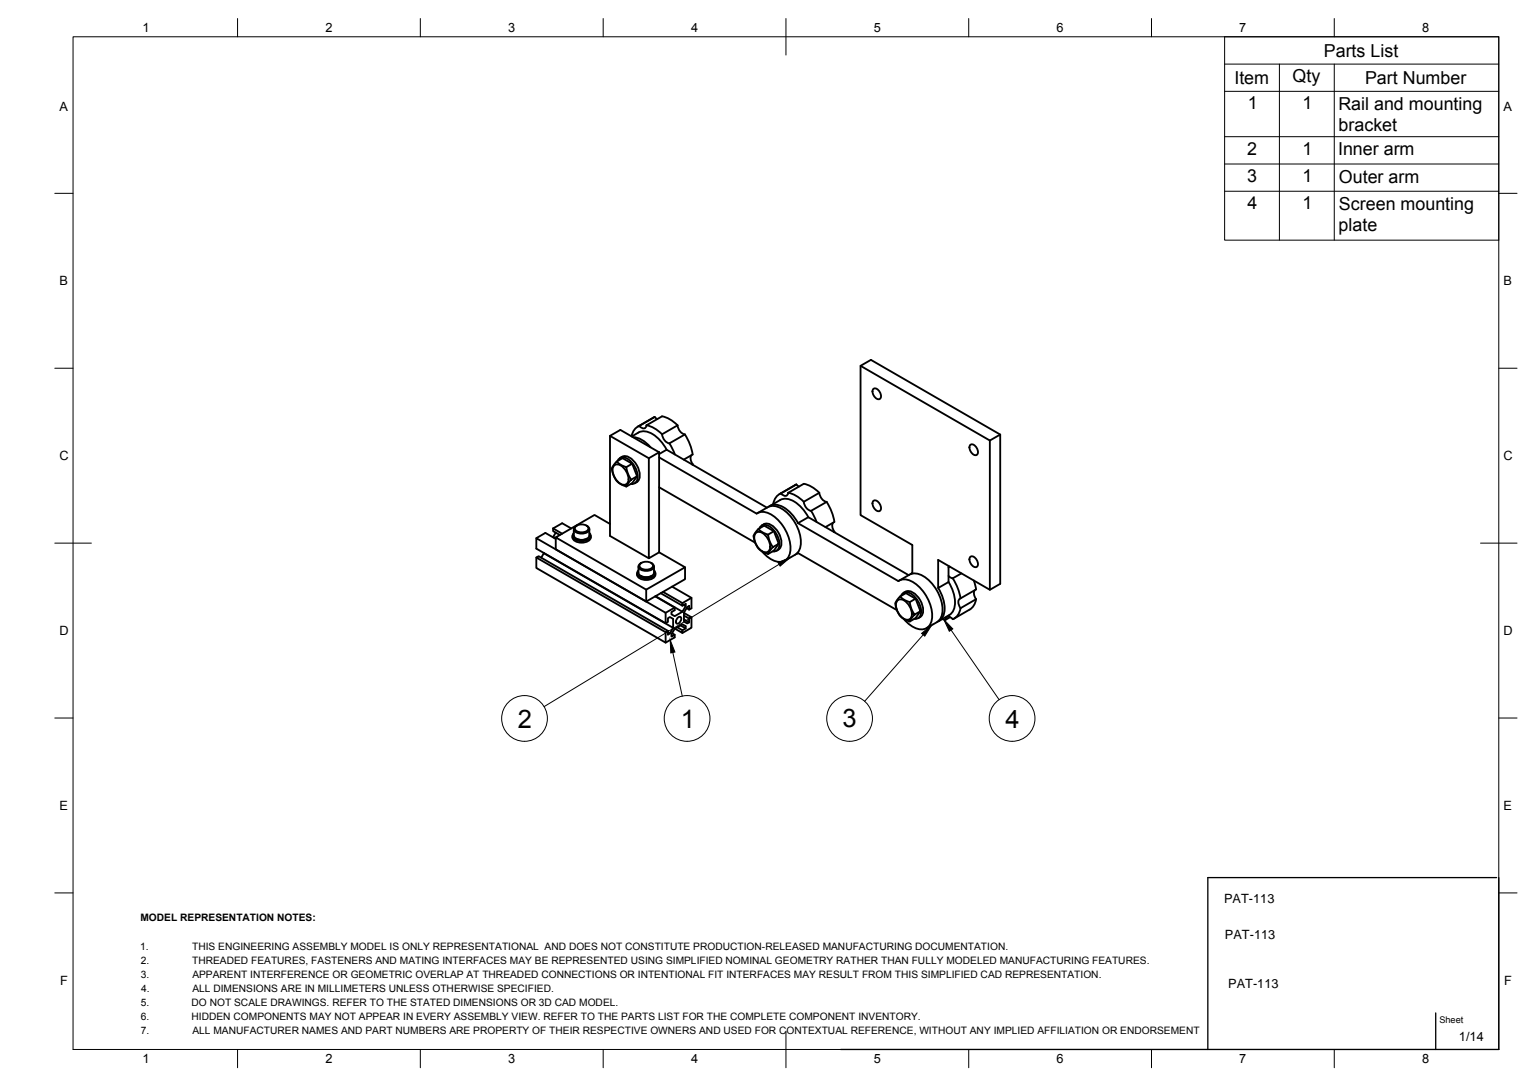
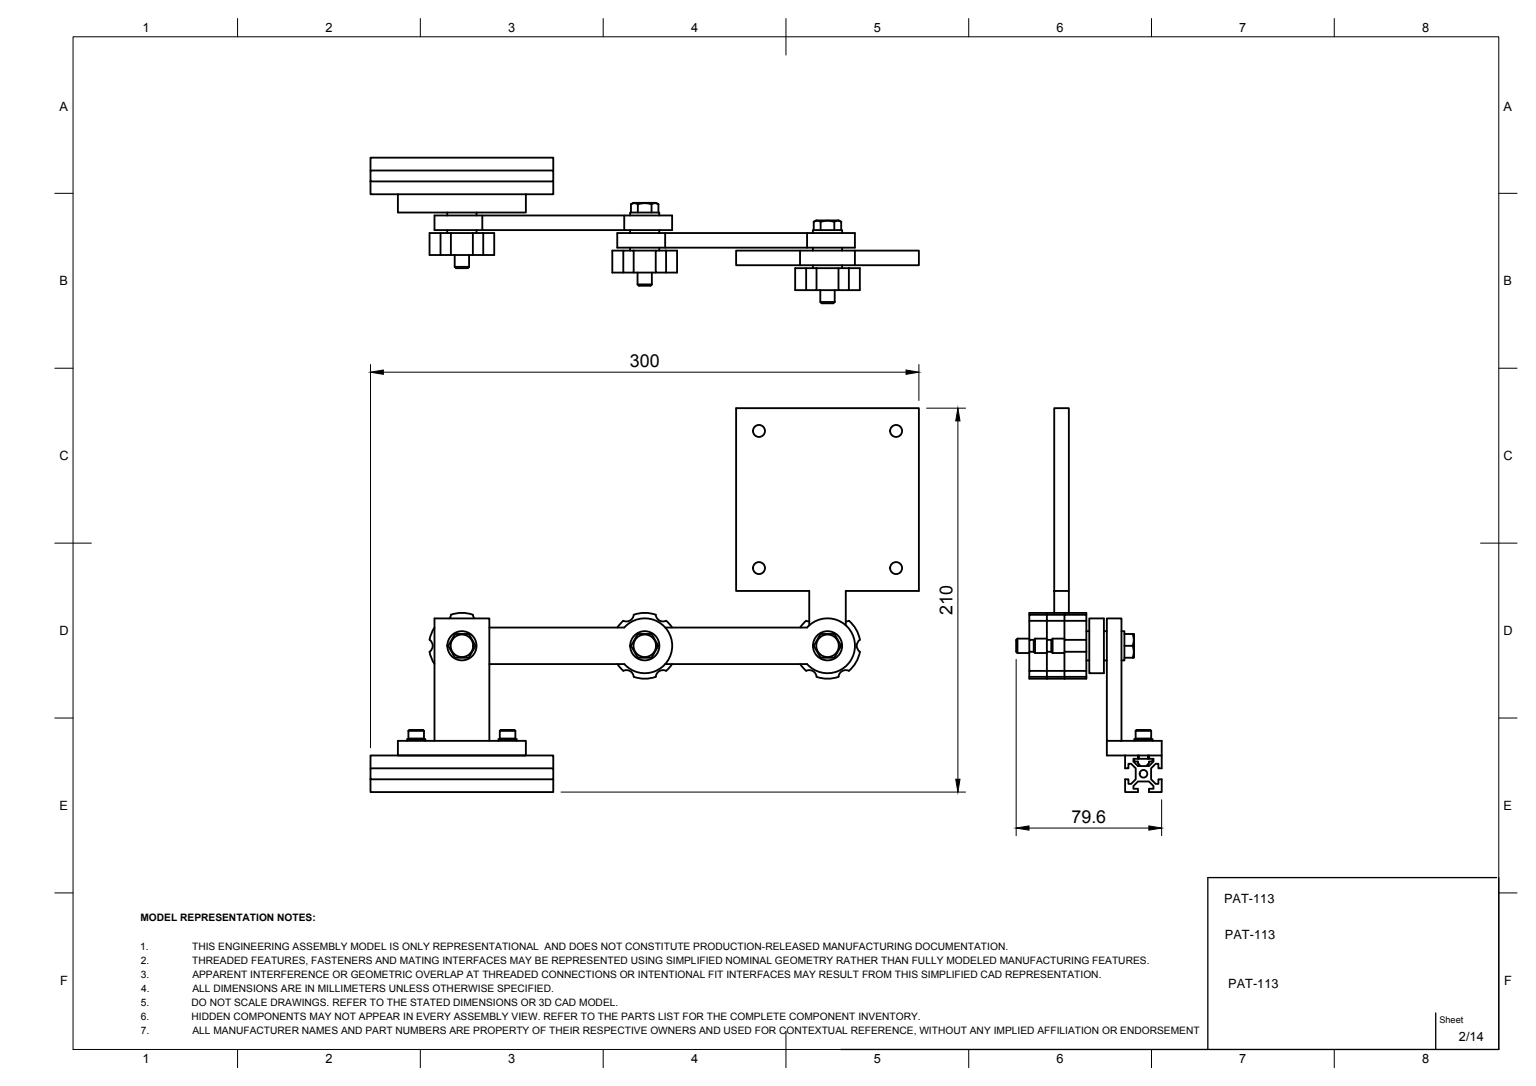
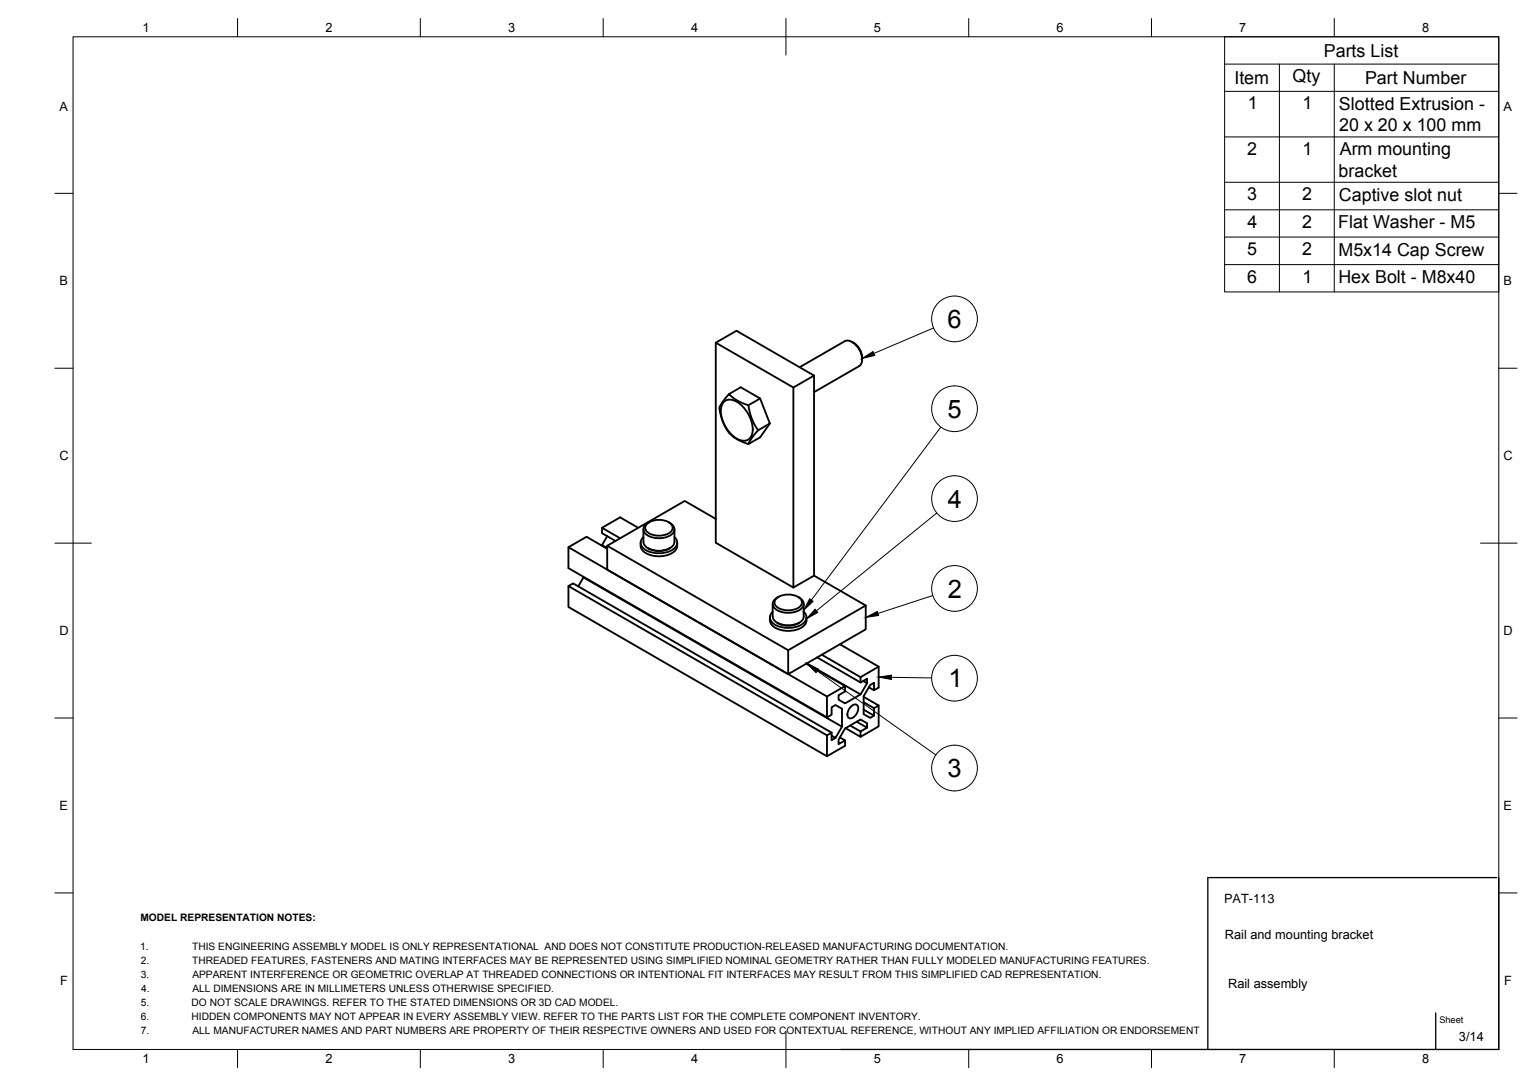
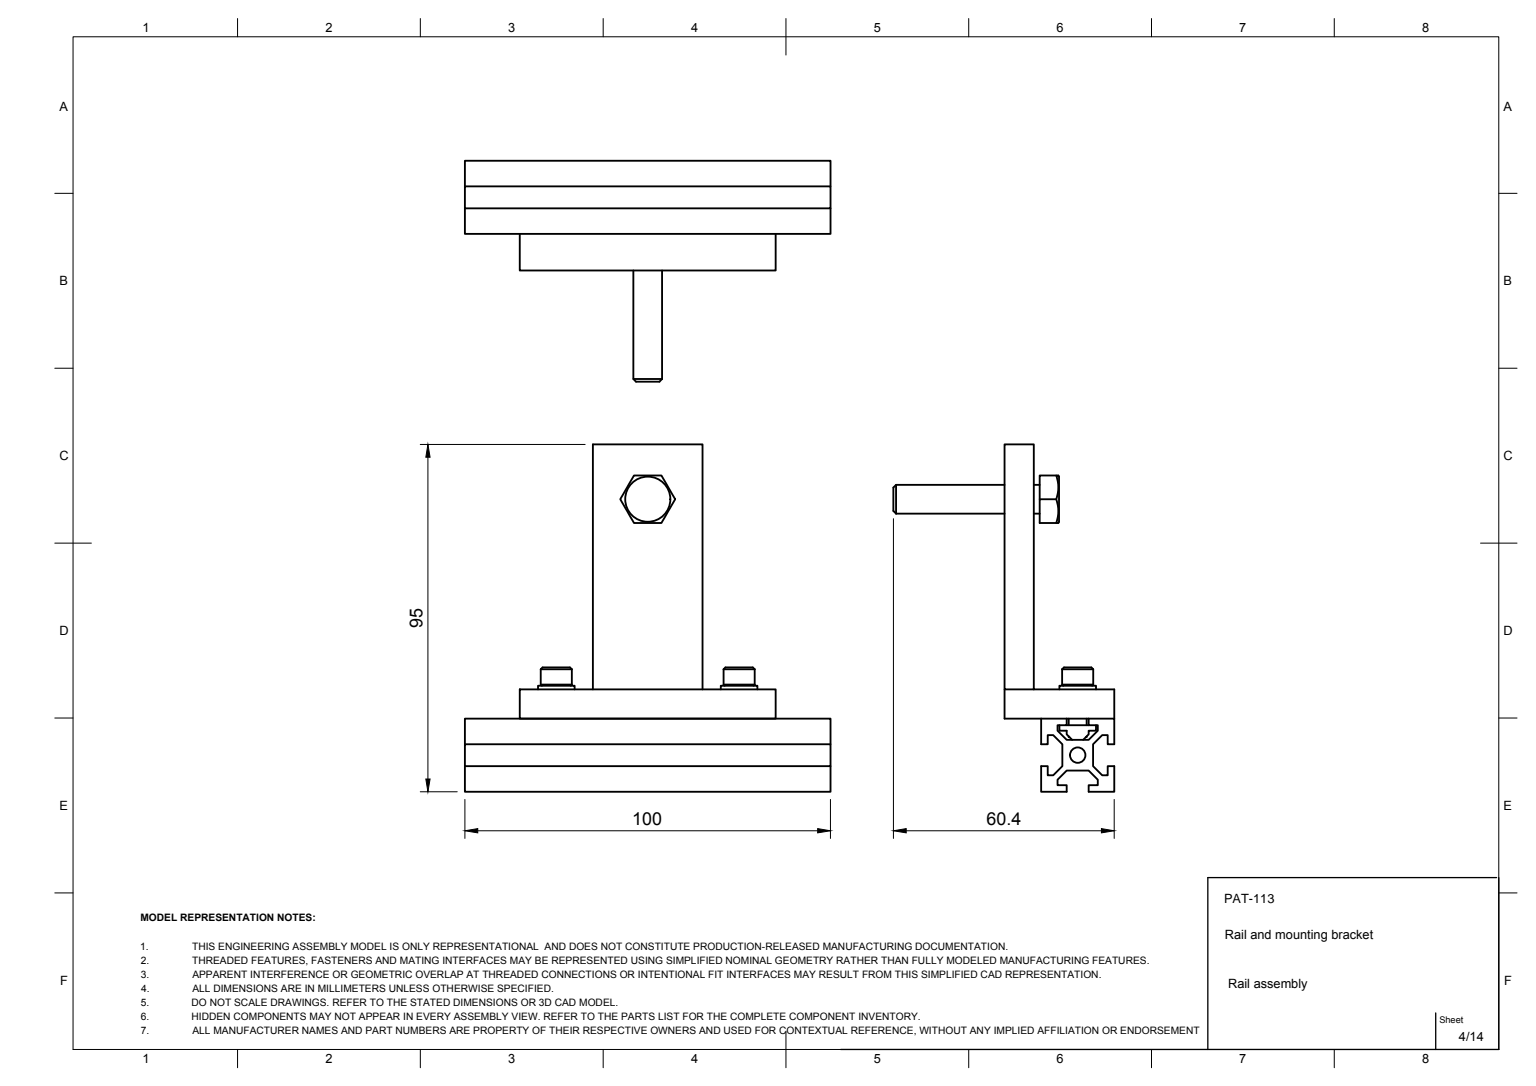
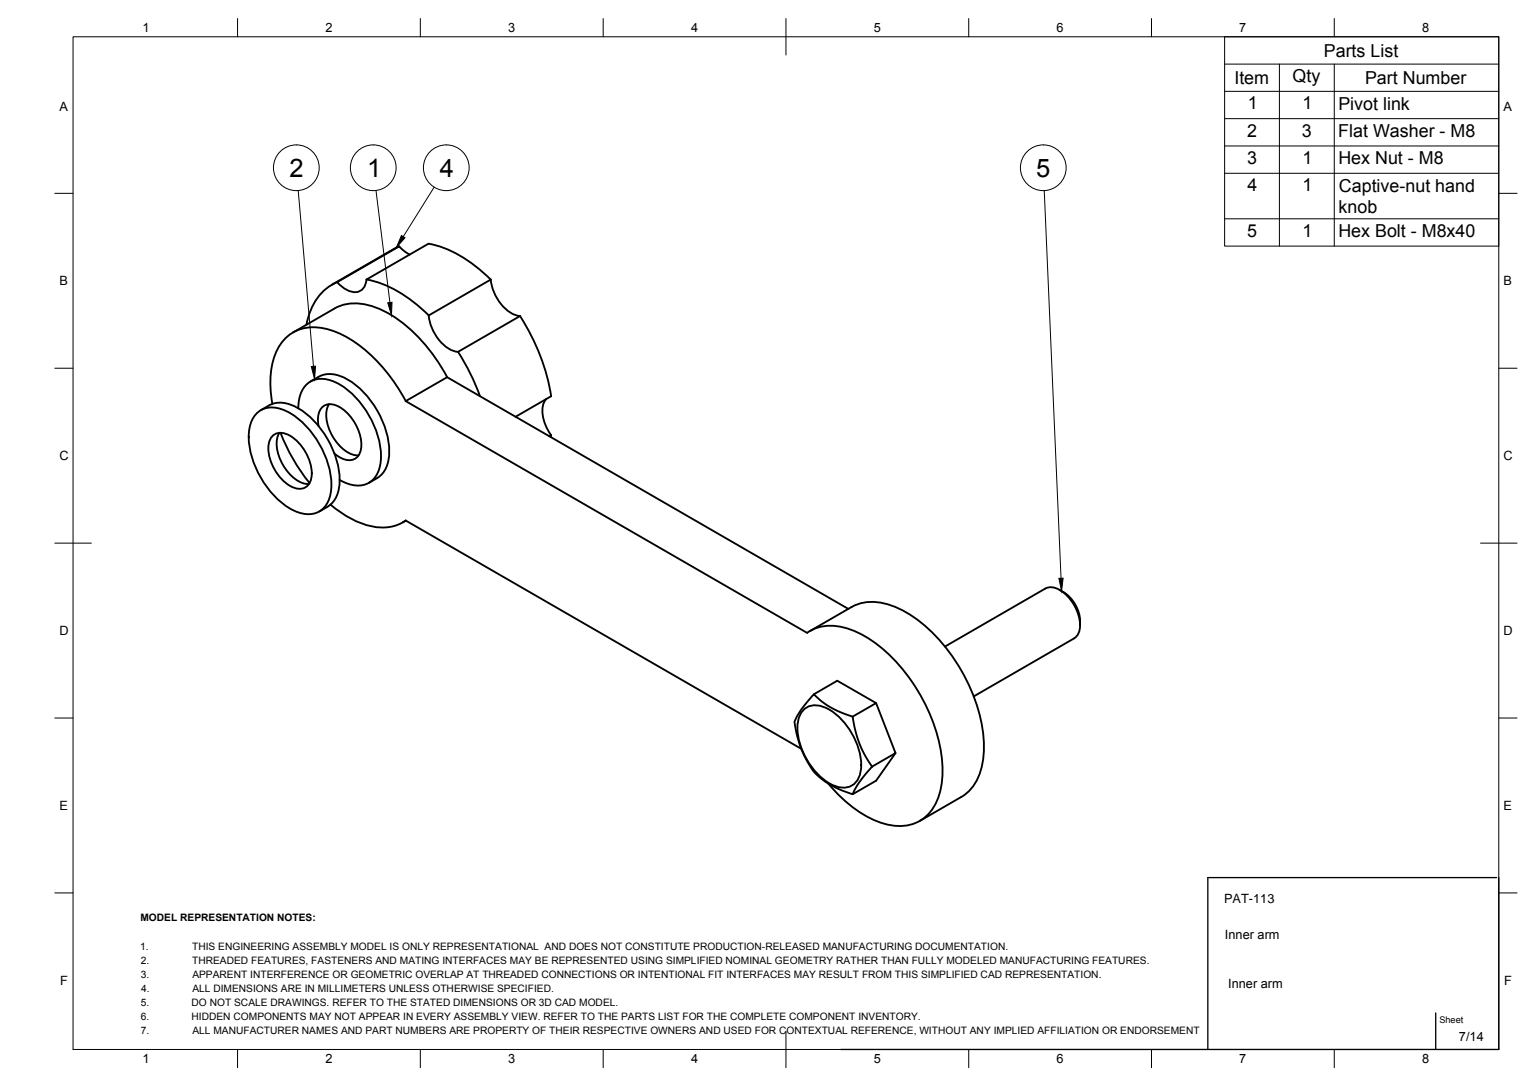
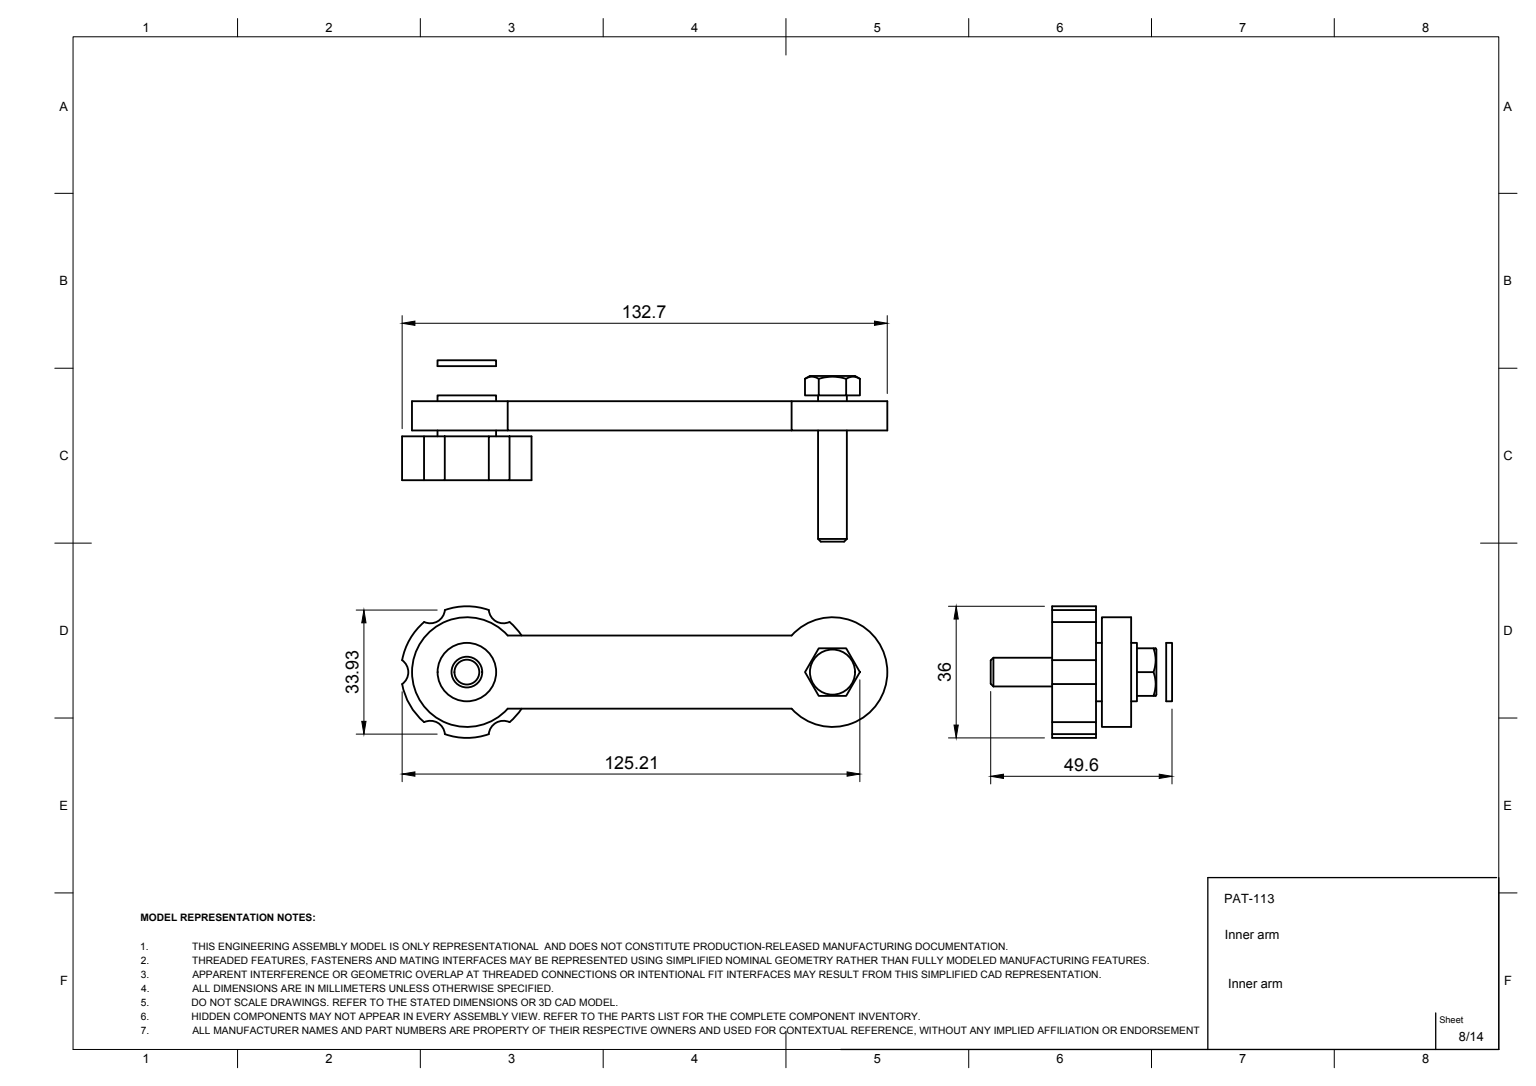
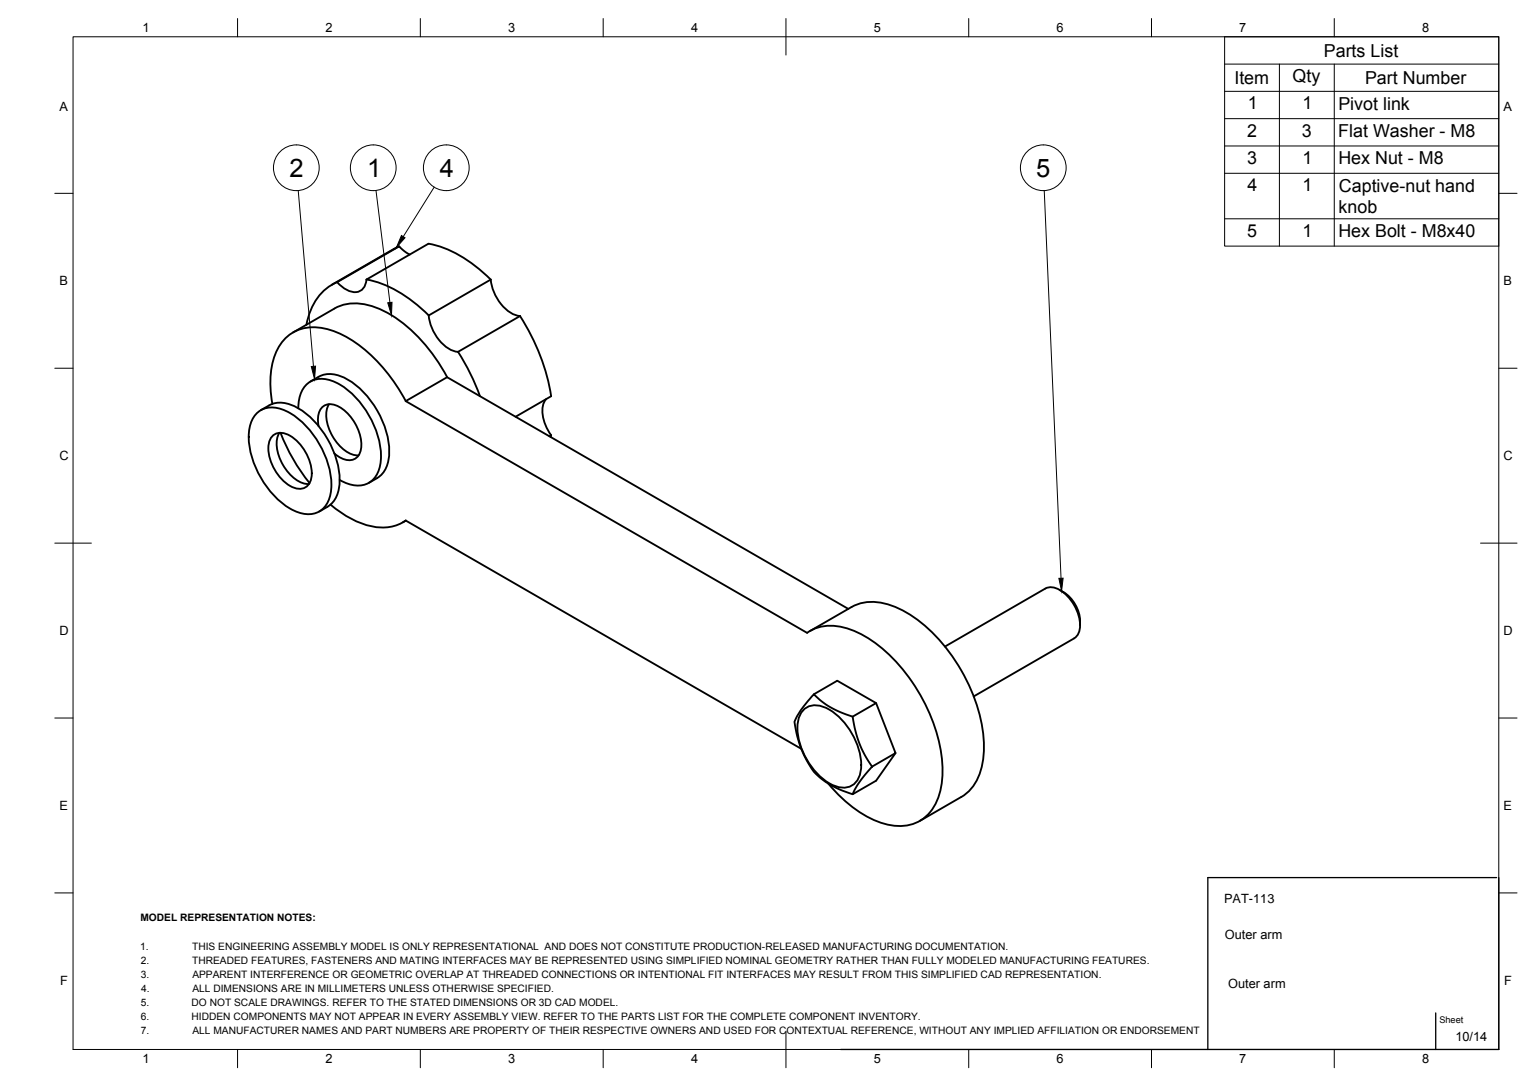
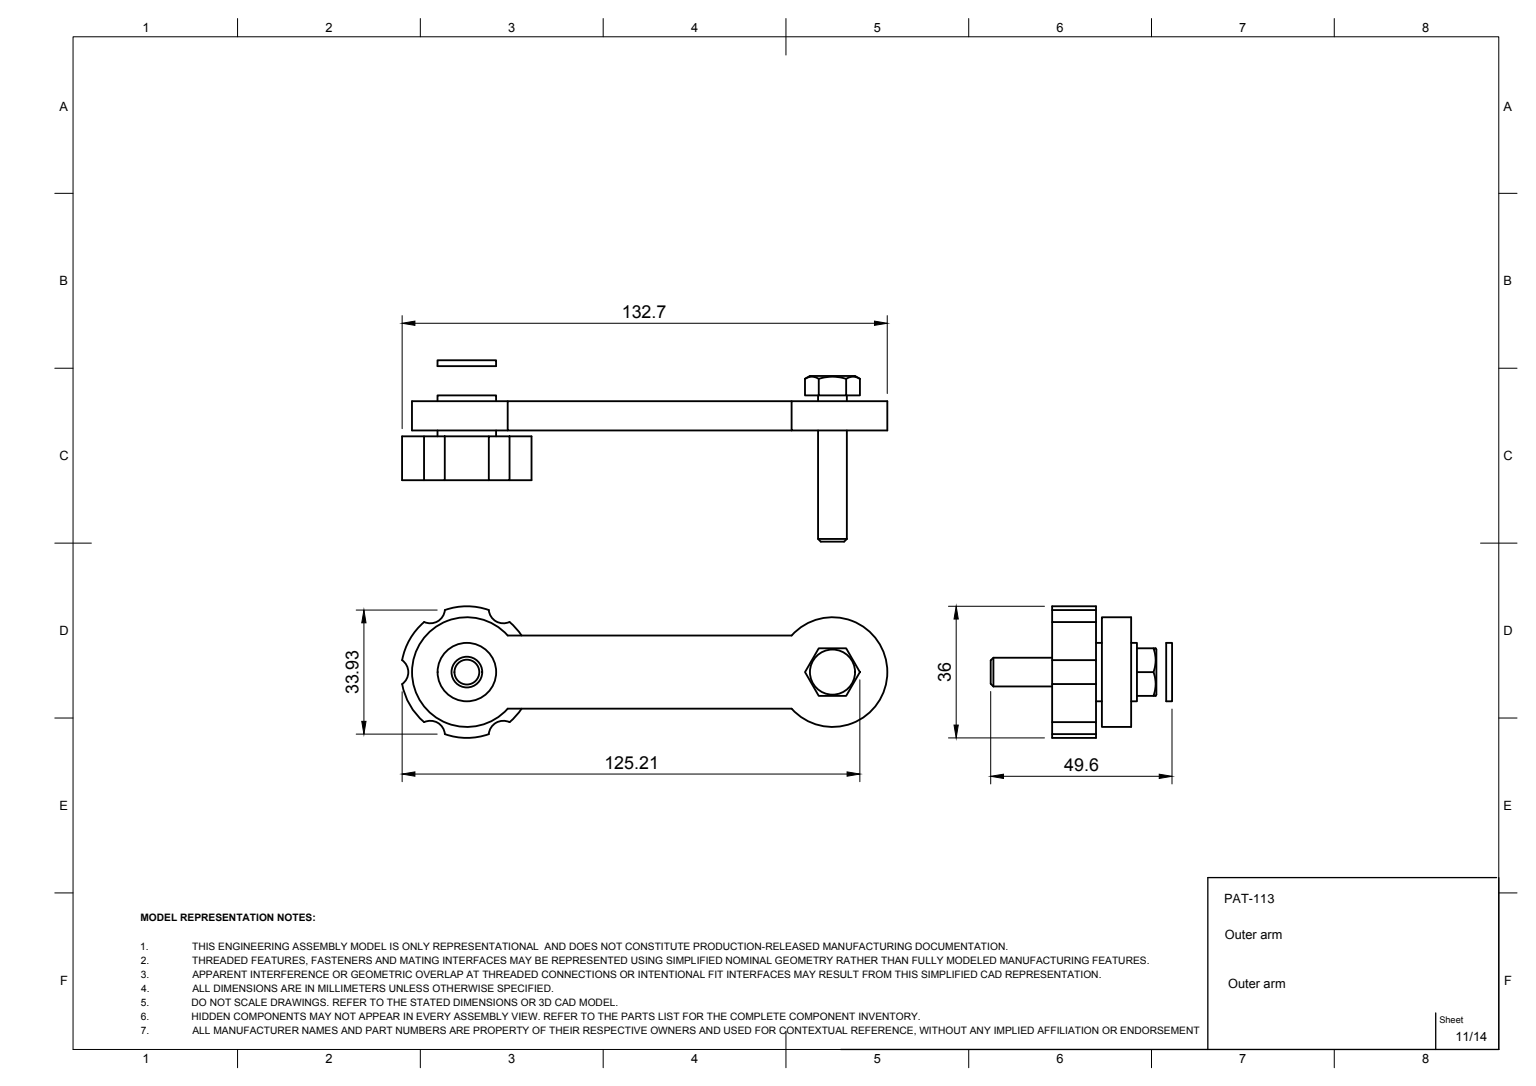
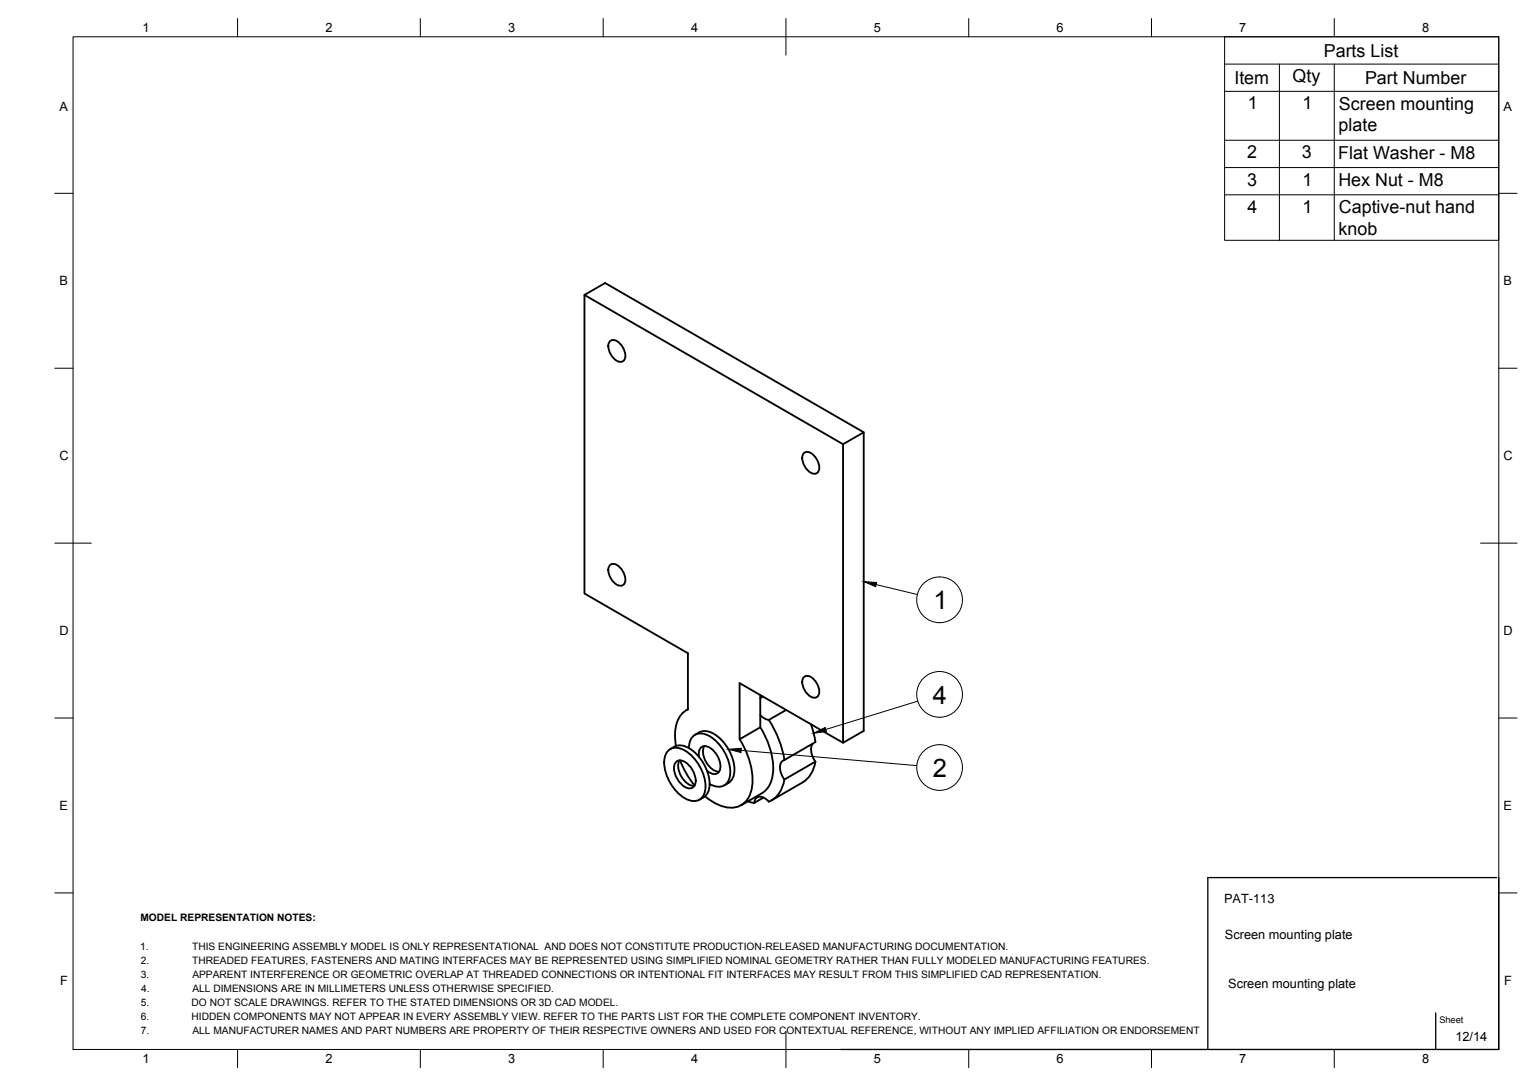
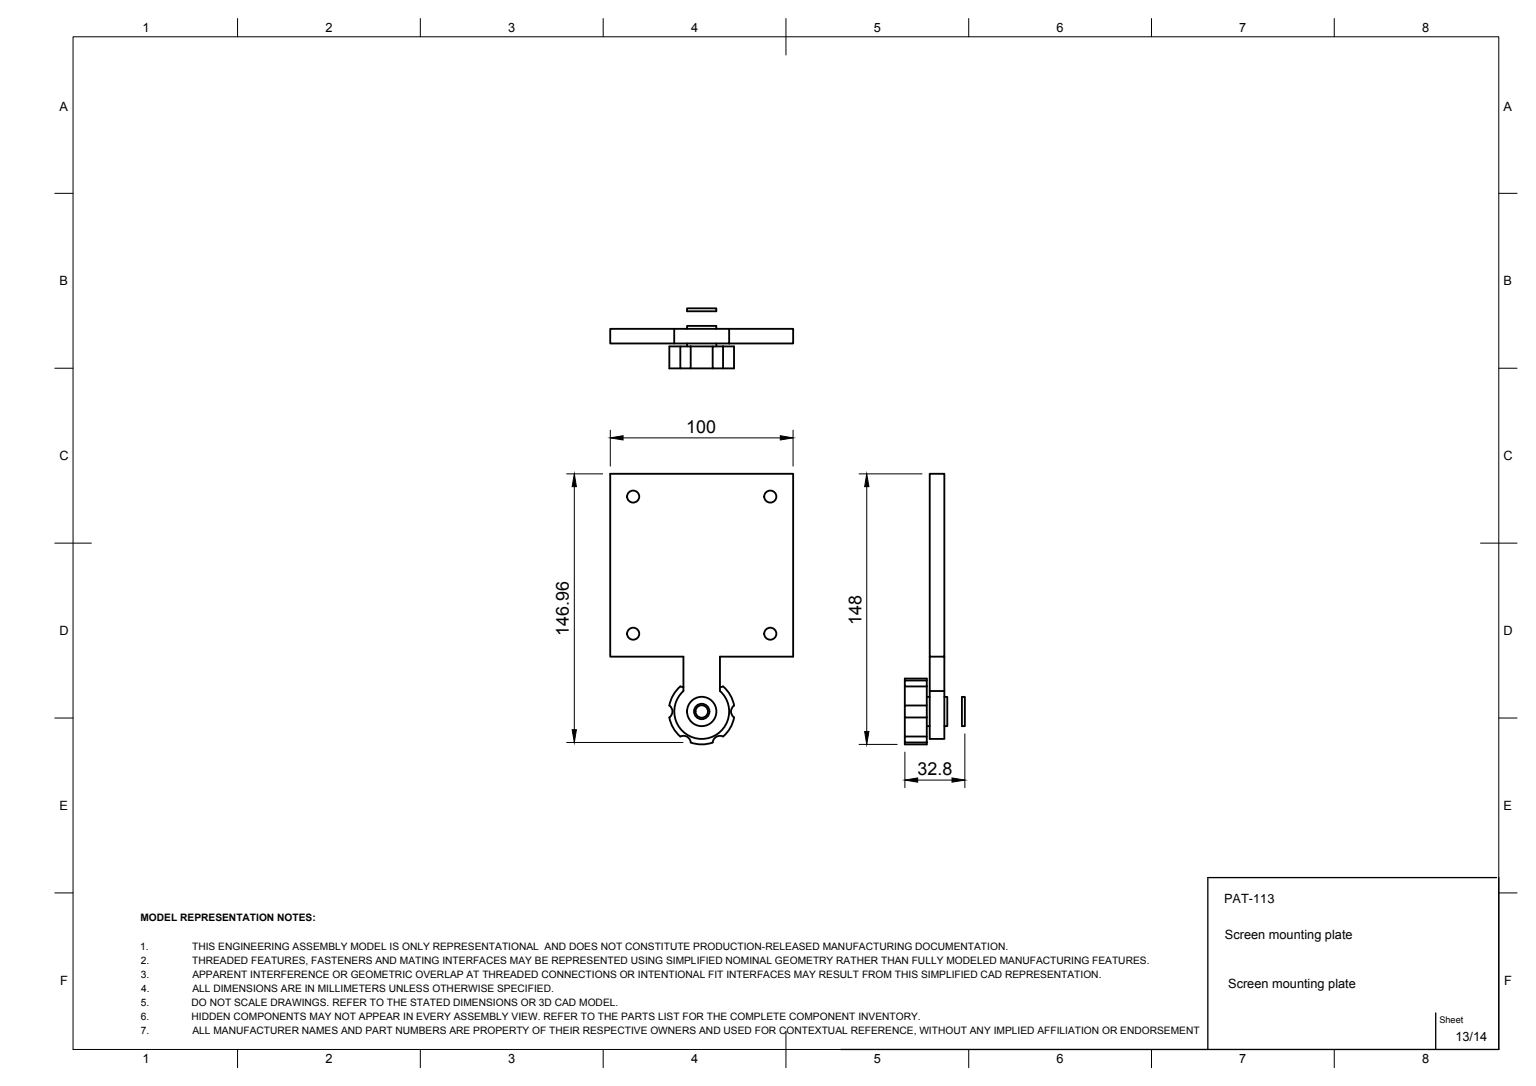
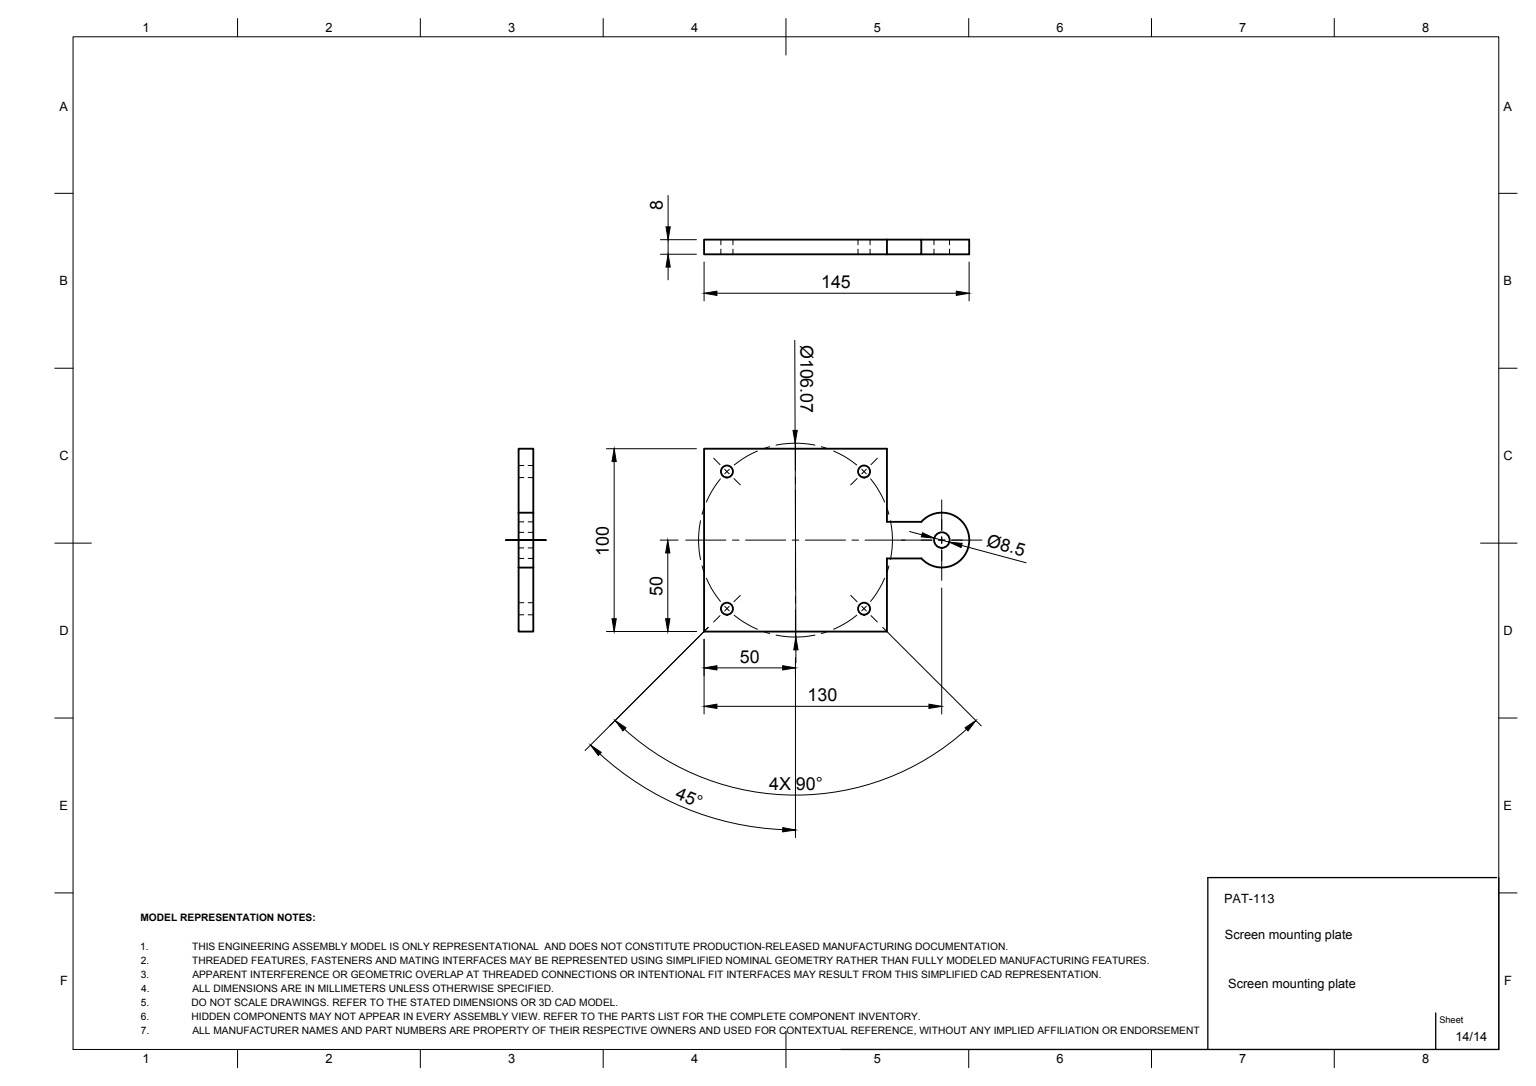
ISO-10303-21;
HEADER;
/* Generated by software containing ST-Developer
 * from STEP Tools, Inc. (www.steptools.com) 
 */

FILE_DESCRIPTION(
/* description */ ('Two-link friction support arm'),
/* implementation_level */ '2;1');

FILE_NAME(
/* name */ 'PAT-113',
/* time_stamp */ '2026-10-27T20:01:49-07:00',
/* author */ (''),
/* organization */ (''),
/* preprocessor_version */ 'ST-DEVELOPER v20.2',
/* originating_system */ 'Autodesk Translation Framework v15.17.0.0',
/* authorisation */ '');

FILE_SCHEMA (('AUTOMOTIVE_DESIGN { 1 0 10303 214 3 1 1 }'));
ENDSEC;

DATA;
#10=MECHANICAL_DESIGN_GEOMETRIC_PRESENTATION_REPRESENTATION('',(#195,#196,
#197,#198,#199,#200,#201,#202,#203,#204,#205),#5492);
#11=ITEM_DEFINED_TRANSFORMATION($,$,#3307,#3469);
#12=ITEM_DEFINED_TRANSFORMATION($,$,#3327,#3470);
#13=ITEM_DEFINED_TRANSFORMATION($,$,#3377,#3471);
#14=ITEM_DEFINED_TRANSFORMATION($,$,#3398,#3472);
#15=ITEM_DEFINED_TRANSFORMATION($,$,#3409,#3473);
#16=ITEM_DEFINED_TRANSFORMATION($,$,#3377,#3474);
#17=ITEM_DEFINED_TRANSFORMATION($,$,#3398,#3475);
#18=ITEM_DEFINED_TRANSFORMATION($,$,#3409,#3476);
#19=ITEM_DEFINED_TRANSFORMATION($,$,#3452,#3477);
#20=ITEM_DEFINED_TRANSFORMATION($,$,#3435,#3581);
#21=ITEM_DEFINED_TRANSFORMATION($,$,#3507,#3582);
#22=ITEM_DEFINED_TRANSFORMATION($,$,#3507,#3583);
#23=ITEM_DEFINED_TRANSFORMATION($,$,#3507,#3584);
#24=ITEM_DEFINED_TRANSFORMATION($,$,#3516,#3585);
#25=ITEM_DEFINED_TRANSFORMATION($,$,#3532,#3586);
#26=ITEM_DEFINED_TRANSFORMATION($,$,#3452,#3587);
#27=ITEM_DEFINED_TRANSFORMATION($,$,#3435,#3588);
#28=ITEM_DEFINED_TRANSFORMATION($,$,#3507,#3589);
#29=ITEM_DEFINED_TRANSFORMATION($,$,#3507,#3590);
#30=ITEM_DEFINED_TRANSFORMATION($,$,#3507,#3591);
#31=ITEM_DEFINED_TRANSFORMATION($,$,#3516,#3592);
#32=ITEM_DEFINED_TRANSFORMATION($,$,#3532,#3593);
#33=ITEM_DEFINED_TRANSFORMATION($,$,#3452,#3594);
#34=ITEM_DEFINED_TRANSFORMATION($,$,#3479,#3595);
#35=ITEM_DEFINED_TRANSFORMATION($,$,#3507,#3596);
#36=ITEM_DEFINED_TRANSFORMATION($,$,#3507,#3597);
#37=ITEM_DEFINED_TRANSFORMATION($,$,#3507,#3598);
#38=ITEM_DEFINED_TRANSFORMATION($,$,#3516,#3599);
#39=ITEM_DEFINED_TRANSFORMATION($,$,#3532,#3600);
#40=ITEM_DEFINED_TRANSFORMATION($,$,#3306,#3601);
#41=ITEM_DEFINED_TRANSFORMATION($,$,#3433,#3602);
#42=ITEM_DEFINED_TRANSFORMATION($,$,#3434,#3603);
#43=ITEM_DEFINED_TRANSFORMATION($,$,#3478,#3604);
#44=(
REPRESENTATION_RELATIONSHIP($,$,#5564,#5563)
REPRESENTATION_RELATIONSHIP_WITH_TRANSFORMATION(#11)
SHAPE_REPRESENTATION_RELATIONSHIP()
);
#45=(
REPRESENTATION_RELATIONSHIP($,$,#5565,#5563)
REPRESENTATION_RELATIONSHIP_WITH_TRANSFORMATION(#12)
SHAPE_REPRESENTATION_RELATIONSHIP()
);
#46=(
REPRESENTATION_RELATIONSHIP($,$,#5566,#5563)
REPRESENTATION_RELATIONSHIP_WITH_TRANSFORMATION(#13)
SHAPE_REPRESENTATION_RELATIONSHIP()
);
#47=(
REPRESENTATION_RELATIONSHIP($,$,#5567,#5563)
REPRESENTATION_RELATIONSHIP_WITH_TRANSFORMATION(#14)
SHAPE_REPRESENTATION_RELATIONSHIP()
);
#48=(
REPRESENTATION_RELATIONSHIP($,$,#5568,#5563)
REPRESENTATION_RELATIONSHIP_WITH_TRANSFORMATION(#15)
SHAPE_REPRESENTATION_RELATIONSHIP()
);
#49=(
REPRESENTATION_RELATIONSHIP($,$,#5566,#5563)
REPRESENTATION_RELATIONSHIP_WITH_TRANSFORMATION(#16)
SHAPE_REPRESENTATION_RELATIONSHIP()
);
#50=(
REPRESENTATION_RELATIONSHIP($,$,#5567,#5563)
REPRESENTATION_RELATIONSHIP_WITH_TRANSFORMATION(#17)
SHAPE_REPRESENTATION_RELATIONSHIP()
);
#51=(
REPRESENTATION_RELATIONSHIP($,$,#5568,#5563)
REPRESENTATION_RELATIONSHIP_WITH_TRANSFORMATION(#18)
SHAPE_REPRESENTATION_RELATIONSHIP()
);
#52=(
REPRESENTATION_RELATIONSHIP($,$,#5572,#5563)
REPRESENTATION_RELATIONSHIP_WITH_TRANSFORMATION(#19)
SHAPE_REPRESENTATION_RELATIONSHIP()
);
#53=(
REPRESENTATION_RELATIONSHIP($,$,#5571,#5569)
REPRESENTATION_RELATIONSHIP_WITH_TRANSFORMATION(#20)
SHAPE_REPRESENTATION_RELATIONSHIP()
);
#54=(
REPRESENTATION_RELATIONSHIP($,$,#5575,#5569)
REPRESENTATION_RELATIONSHIP_WITH_TRANSFORMATION(#21)
SHAPE_REPRESENTATION_RELATIONSHIP()
);
#55=(
REPRESENTATION_RELATIONSHIP($,$,#5575,#5569)
REPRESENTATION_RELATIONSHIP_WITH_TRANSFORMATION(#22)
SHAPE_REPRESENTATION_RELATIONSHIP()
);
#56=(
REPRESENTATION_RELATIONSHIP($,$,#5575,#5569)
REPRESENTATION_RELATIONSHIP_WITH_TRANSFORMATION(#23)
SHAPE_REPRESENTATION_RELATIONSHIP()
);
#57=(
REPRESENTATION_RELATIONSHIP($,$,#5576,#5569)
REPRESENTATION_RELATIONSHIP_WITH_TRANSFORMATION(#24)
SHAPE_REPRESENTATION_RELATIONSHIP()
);
#58=(
REPRESENTATION_RELATIONSHIP($,$,#5577,#5569)
REPRESENTATION_RELATIONSHIP_WITH_TRANSFORMATION(#25)
SHAPE_REPRESENTATION_RELATIONSHIP()
);
#59=(
REPRESENTATION_RELATIONSHIP($,$,#5572,#5569)
REPRESENTATION_RELATIONSHIP_WITH_TRANSFORMATION(#26)
SHAPE_REPRESENTATION_RELATIONSHIP()
);
#60=(
REPRESENTATION_RELATIONSHIP($,$,#5571,#5570)
REPRESENTATION_RELATIONSHIP_WITH_TRANSFORMATION(#27)
SHAPE_REPRESENTATION_RELATIONSHIP()
);
#61=(
REPRESENTATION_RELATIONSHIP($,$,#5575,#5570)
REPRESENTATION_RELATIONSHIP_WITH_TRANSFORMATION(#28)
SHAPE_REPRESENTATION_RELATIONSHIP()
);
#62=(
REPRESENTATION_RELATIONSHIP($,$,#5575,#5570)
REPRESENTATION_RELATIONSHIP_WITH_TRANSFORMATION(#29)
SHAPE_REPRESENTATION_RELATIONSHIP()
);
#63=(
REPRESENTATION_RELATIONSHIP($,$,#5575,#5570)
REPRESENTATION_RELATIONSHIP_WITH_TRANSFORMATION(#30)
SHAPE_REPRESENTATION_RELATIONSHIP()
);
#64=(
REPRESENTATION_RELATIONSHIP($,$,#5576,#5570)
REPRESENTATION_RELATIONSHIP_WITH_TRANSFORMATION(#31)
SHAPE_REPRESENTATION_RELATIONSHIP()
);
#65=(
REPRESENTATION_RELATIONSHIP($,$,#5577,#5570)
REPRESENTATION_RELATIONSHIP_WITH_TRANSFORMATION(#32)
SHAPE_REPRESENTATION_RELATIONSHIP()
);
#66=(
REPRESENTATION_RELATIONSHIP($,$,#5572,#5570)
REPRESENTATION_RELATIONSHIP_WITH_TRANSFORMATION(#33)
SHAPE_REPRESENTATION_RELATIONSHIP()
);
#67=(
REPRESENTATION_RELATIONSHIP($,$,#5574,#5573)
REPRESENTATION_RELATIONSHIP_WITH_TRANSFORMATION(#34)
SHAPE_REPRESENTATION_RELATIONSHIP()
);
#68=(
REPRESENTATION_RELATIONSHIP($,$,#5575,#5573)
REPRESENTATION_RELATIONSHIP_WITH_TRANSFORMATION(#35)
SHAPE_REPRESENTATION_RELATIONSHIP()
);
#69=(
REPRESENTATION_RELATIONSHIP($,$,#5575,#5573)
REPRESENTATION_RELATIONSHIP_WITH_TRANSFORMATION(#36)
SHAPE_REPRESENTATION_RELATIONSHIP()
);
#70=(
REPRESENTATION_RELATIONSHIP($,$,#5575,#5573)
REPRESENTATION_RELATIONSHIP_WITH_TRANSFORMATION(#37)
SHAPE_REPRESENTATION_RELATIONSHIP()
);
#71=(
REPRESENTATION_RELATIONSHIP($,$,#5576,#5573)
REPRESENTATION_RELATIONSHIP_WITH_TRANSFORMATION(#38)
SHAPE_REPRESENTATION_RELATIONSHIP()
);
#72=(
REPRESENTATION_RELATIONSHIP($,$,#5577,#5573)
REPRESENTATION_RELATIONSHIP_WITH_TRANSFORMATION(#39)
SHAPE_REPRESENTATION_RELATIONSHIP()
);
#73=(
REPRESENTATION_RELATIONSHIP($,$,#5563,#5562)
REPRESENTATION_RELATIONSHIP_WITH_TRANSFORMATION(#40)
SHAPE_REPRESENTATION_RELATIONSHIP()
);
#74=(
REPRESENTATION_RELATIONSHIP($,$,#5569,#5562)
REPRESENTATION_RELATIONSHIP_WITH_TRANSFORMATION(#41)
SHAPE_REPRESENTATION_RELATIONSHIP()
);
#75=(
REPRESENTATION_RELATIONSHIP($,$,#5570,#5562)
REPRESENTATION_RELATIONSHIP_WITH_TRANSFORMATION(#42)
SHAPE_REPRESENTATION_RELATIONSHIP()
);
#76=(
REPRESENTATION_RELATIONSHIP($,$,#5573,#5562)
REPRESENTATION_RELATIONSHIP_WITH_TRANSFORMATION(#43)
SHAPE_REPRESENTATION_RELATIONSHIP()
);
#77=CONTEXT_DEPENDENT_SHAPE_REPRESENTATION(#44,#5524);
#78=CONTEXT_DEPENDENT_SHAPE_REPRESENTATION(#45,#5525);
#79=CONTEXT_DEPENDENT_SHAPE_REPRESENTATION(#46,#5526);
#80=CONTEXT_DEPENDENT_SHAPE_REPRESENTATION(#47,#5527);
#81=CONTEXT_DEPENDENT_SHAPE_REPRESENTATION(#48,#5528);
#82=CONTEXT_DEPENDENT_SHAPE_REPRESENTATION(#49,#5529);
#83=CONTEXT_DEPENDENT_SHAPE_REPRESENTATION(#50,#5530);
#84=CONTEXT_DEPENDENT_SHAPE_REPRESENTATION(#51,#5531);
#85=CONTEXT_DEPENDENT_SHAPE_REPRESENTATION(#52,#5532);
#86=CONTEXT_DEPENDENT_SHAPE_REPRESENTATION(#53,#5538);
#87=CONTEXT_DEPENDENT_SHAPE_REPRESENTATION(#54,#5539);
#88=CONTEXT_DEPENDENT_SHAPE_REPRESENTATION(#55,#5540);
#89=CONTEXT_DEPENDENT_SHAPE_REPRESENTATION(#56,#5541);
#90=CONTEXT_DEPENDENT_SHAPE_REPRESENTATION(#57,#5542);
#91=CONTEXT_DEPENDENT_SHAPE_REPRESENTATION(#58,#5543);
#92=CONTEXT_DEPENDENT_SHAPE_REPRESENTATION(#59,#5544);
#93=CONTEXT_DEPENDENT_SHAPE_REPRESENTATION(#60,#5545);
#94=CONTEXT_DEPENDENT_SHAPE_REPRESENTATION(#61,#5546);
#95=CONTEXT_DEPENDENT_SHAPE_REPRESENTATION(#62,#5547);
#96=CONTEXT_DEPENDENT_SHAPE_REPRESENTATION(#63,#5548);
#97=CONTEXT_DEPENDENT_SHAPE_REPRESENTATION(#64,#5549);
#98=CONTEXT_DEPENDENT_SHAPE_REPRESENTATION(#65,#5550);
#99=CONTEXT_DEPENDENT_SHAPE_REPRESENTATION(#66,#5551);
#100=CONTEXT_DEPENDENT_SHAPE_REPRESENTATION(#67,#5552);
#101=CONTEXT_DEPENDENT_SHAPE_REPRESENTATION(#68,#5553);
#102=CONTEXT_DEPENDENT_SHAPE_REPRESENTATION(#69,#5554);
#103=CONTEXT_DEPENDENT_SHAPE_REPRESENTATION(#70,#5555);
#104=CONTEXT_DEPENDENT_SHAPE_REPRESENTATION(#71,#5556);
#105=CONTEXT_DEPENDENT_SHAPE_REPRESENTATION(#72,#5557);
#106=CONTEXT_DEPENDENT_SHAPE_REPRESENTATION(#73,#5558);
#107=CONTEXT_DEPENDENT_SHAPE_REPRESENTATION(#74,#5559);
#108=CONTEXT_DEPENDENT_SHAPE_REPRESENTATION(#75,#5560);
#109=CONTEXT_DEPENDENT_SHAPE_REPRESENTATION(#76,#5561);
#110=NEXT_ASSEMBLY_USAGE_OCCURRENCE('Arm mounting bracket:1',
'Arm mounting bracket:1','Arm mounting bracket:1',#5580,#5581,
'Arm mounting bracket:1');
#111=NEXT_ASSEMBLY_USAGE_OCCURRENCE(
'Slotted Extrusion - 20 x 20 x 100 mm:2',
'Slotted Extrusion - 20 x 20 x 100 mm:2',
'Slotted Extrusion - 20 x 20 x 100 mm:2',#5580,#5582,
'Slotted Extrusion - 20 x 20 x 100 mm:2');
#112=NEXT_ASSEMBLY_USAGE_OCCURRENCE('Captive slot nut:2',
'Captive slot nut:2','Captive slot nut:2',#5580,#5583,
'Captive slot nut:2');
#113=NEXT_ASSEMBLY_USAGE_OCCURRENCE('Flat Washer - M5:2',
'Flat Washer - M5:2','Flat Washer - M5:2',#5580,#5584,
'Flat Washer - M5:2');
#114=NEXT_ASSEMBLY_USAGE_OCCURRENCE('M5x14 Cap Screw:2',
'M5x14 Cap Screw:2','M5x14 Cap Screw:2',#5580,#5585,'M5x14 Cap Screw:2');
#115=NEXT_ASSEMBLY_USAGE_OCCURRENCE('Captive slot nut:3',
'Captive slot nut:3','Captive slot nut:3',#5580,#5583,
'Captive slot nut:3');
#116=NEXT_ASSEMBLY_USAGE_OCCURRENCE('Flat Washer - M5:3',
'Flat Washer - M5:3','Flat Washer - M5:3',#5580,#5584,
'Flat Washer - M5:3');
#117=NEXT_ASSEMBLY_USAGE_OCCURRENCE('M5x14 Cap Screw:3',
'M5x14 Cap Screw:3','M5x14 Cap Screw:3',#5580,#5585,'M5x14 Cap Screw:3');
#118=NEXT_ASSEMBLY_USAGE_OCCURRENCE('Hex Bolt - M8x40:2',
'Hex Bolt - M8x40:2','Hex Bolt - M8x40:2',#5580,#5589,
'Hex Bolt - M8x40:2');
#119=NEXT_ASSEMBLY_USAGE_OCCURRENCE('Pivot link:1','Pivot link:1',
'Pivot link:1',#5586,#5588,'Pivot link:1');
#120=NEXT_ASSEMBLY_USAGE_OCCURRENCE('Flat Washer - M8:2',
'Flat Washer - M8:2','Flat Washer - M8:2',#5586,#5592,
'Flat Washer - M8:2');
#121=NEXT_ASSEMBLY_USAGE_OCCURRENCE('Flat Washer - M8:3',
'Flat Washer - M8:3','Flat Washer - M8:3',#5586,#5592,
'Flat Washer - M8:3');
#122=NEXT_ASSEMBLY_USAGE_OCCURRENCE('Flat Washer - M8:4',
'Flat Washer - M8:4','Flat Washer - M8:4',#5586,#5592,
'Flat Washer - M8:4');
#123=NEXT_ASSEMBLY_USAGE_OCCURRENCE('Hex Nut - M8:2','Hex Nut - M8:2',
'Hex Nut - M8:2',#5586,#5593,'Hex Nut - M8:2');
#124=NEXT_ASSEMBLY_USAGE_OCCURRENCE('Captive-nut hand knob:2',
'Captive-nut hand knob:2','Captive-nut hand knob:2',#5586,#5594,
'Captive-nut hand knob:2');
#125=NEXT_ASSEMBLY_USAGE_OCCURRENCE('Hex Bolt - M8x40:3',
'Hex Bolt - M8x40:3','Hex Bolt - M8x40:3',#5586,#5589,
'Hex Bolt - M8x40:3');
#126=NEXT_ASSEMBLY_USAGE_OCCURRENCE('Pivot link:2','Pivot link:2',
'Pivot link:2',#5587,#5588,'Pivot link:2');
#127=NEXT_ASSEMBLY_USAGE_OCCURRENCE('Flat Washer - M8:5',
'Flat Washer - M8:5','Flat Washer - M8:5',#5587,#5592,
'Flat Washer - M8:5');
#128=NEXT_ASSEMBLY_USAGE_OCCURRENCE('Flat Washer - M8:6',
'Flat Washer - M8:6','Flat Washer - M8:6',#5587,#5592,
'Flat Washer - M8:6');
#129=NEXT_ASSEMBLY_USAGE_OCCURRENCE('Flat Washer - M8:7',
'Flat Washer - M8:7','Flat Washer - M8:7',#5587,#5592,
'Flat Washer - M8:7');
#130=NEXT_ASSEMBLY_USAGE_OCCURRENCE('Hex Nut - M8:3','Hex Nut - M8:3',
'Hex Nut - M8:3',#5587,#5593,'Hex Nut - M8:3');
#131=NEXT_ASSEMBLY_USAGE_OCCURRENCE('Captive-nut hand knob:3',
'Captive-nut hand knob:3','Captive-nut hand knob:3',#5587,#5594,
'Captive-nut hand knob:3');
#132=NEXT_ASSEMBLY_USAGE_OCCURRENCE('Hex Bolt - M8x40:4',
'Hex Bolt - M8x40:4','Hex Bolt - M8x40:4',#5587,#5589,
'Hex Bolt - M8x40:4');
#133=NEXT_ASSEMBLY_USAGE_OCCURRENCE('Screen mounting plate (1):1',
'Screen mounting plate (1):1','Screen mounting plate (1):1',#5590,#5591,
'Screen mounting plate (1):1');
#134=NEXT_ASSEMBLY_USAGE_OCCURRENCE('Flat Washer - M8:8',
'Flat Washer - M8:8','Flat Washer - M8:8',#5590,#5592,
'Flat Washer - M8:8');
#135=NEXT_ASSEMBLY_USAGE_OCCURRENCE('Flat Washer - M8:9',
'Flat Washer - M8:9','Flat Washer - M8:9',#5590,#5592,
'Flat Washer - M8:9');
#136=NEXT_ASSEMBLY_USAGE_OCCURRENCE('Flat Washer - M8:10',
'Flat Washer - M8:10','Flat Washer - M8:10',#5590,#5592,
'Flat Washer - M8:10');
#137=NEXT_ASSEMBLY_USAGE_OCCURRENCE('Hex Nut - M8:4','Hex Nut - M8:4',
'Hex Nut - M8:4',#5590,#5593,'Hex Nut - M8:4');
#138=NEXT_ASSEMBLY_USAGE_OCCURRENCE('Captive-nut hand knob:4',
'Captive-nut hand knob:4','Captive-nut hand knob:4',#5590,#5594,
'Captive-nut hand knob:4');
#139=NEXT_ASSEMBLY_USAGE_OCCURRENCE('Rail and mounting bracket:1',
'Rail and mounting bracket:1','Rail and mounting bracket:1',#5579,#5580,
'Rail and mounting bracket:1');
#140=NEXT_ASSEMBLY_USAGE_OCCURRENCE('Inner arm:1','Inner arm:1',
'Inner arm:1',#5579,#5586,'Inner arm:1');
#141=NEXT_ASSEMBLY_USAGE_OCCURRENCE('Outer arm:1','Outer arm:1',
'Outer arm:1',#5579,#5587,'Outer arm:1');
#142=NEXT_ASSEMBLY_USAGE_OCCURRENCE('Screen mounting plate:1',
'Screen mounting plate:1','Screen mounting plate:1',#5579,#5590,
'Screen mounting plate:1');
#143=(
BOUNDED_CURVE()
B_SPLINE_CURVE(2,(#5086,#5087,#5088),.UNSPECIFIED.,.F.,.F.)
B_SPLINE_CURVE_WITH_KNOTS((3,3),(0.14973948338295,0.97160236658079),
 .UNSPECIFIED.)
CURVE()
GEOMETRIC_REPRESENTATION_ITEM()
RATIONAL_B_SPLINE_CURVE((1.07140024848292,1.23714644374248,1.07140024848292))
REPRESENTATION_ITEM('')
);
#144=(
BOUNDED_CURVE()
B_SPLINE_CURVE(2,(#5090,#5091,#5092),.UNSPECIFIED.,.F.,.F.)
B_SPLINE_CURVE_WITH_KNOTS((3,3),(0.14973948338295,0.97160236658079),
 .UNSPECIFIED.)
CURVE()
GEOMETRIC_REPRESENTATION_ITEM()
RATIONAL_B_SPLINE_CURVE((1.07140024848292,1.23714644374248,1.07140024848292))
REPRESENTATION_ITEM('')
);
#145=(
BOUNDED_CURVE()
B_SPLINE_CURVE(2,(#5094,#5095,#5096),.UNSPECIFIED.,.F.,.F.)
B_SPLINE_CURVE_WITH_KNOTS((3,3),(0.14973948338295,0.97160236658079),
 .UNSPECIFIED.)
CURVE()
GEOMETRIC_REPRESENTATION_ITEM()
RATIONAL_B_SPLINE_CURVE((1.07140024848292,1.23714644374248,1.07140024848292))
REPRESENTATION_ITEM('')
);
#146=(
BOUNDED_CURVE()
B_SPLINE_CURVE(2,(#5098,#5099,#5100),.UNSPECIFIED.,.F.,.F.)
B_SPLINE_CURVE_WITH_KNOTS((3,3),(0.149739483382949,0.971602366580789),
 .UNSPECIFIED.)
CURVE()
GEOMETRIC_REPRESENTATION_ITEM()
RATIONAL_B_SPLINE_CURVE((1.07140024848292,1.23714644374248,1.07140024848292))
REPRESENTATION_ITEM('')
);
#147=(
BOUNDED_CURVE()
B_SPLINE_CURVE(2,(#5102,#5103,#5104),.UNSPECIFIED.,.F.,.F.)
B_SPLINE_CURVE_WITH_KNOTS((3,3),(0.14973948338295,0.971602366580789),
 .UNSPECIFIED.)
CURVE()
GEOMETRIC_REPRESENTATION_ITEM()
RATIONAL_B_SPLINE_CURVE((1.07140024848292,1.23714644374248,1.07140024848292))
REPRESENTATION_ITEM('')
);
#148=(
BOUNDED_CURVE()
B_SPLINE_CURVE(2,(#5105,#5106,#5107),.UNSPECIFIED.,.F.,.F.)
B_SPLINE_CURVE_WITH_KNOTS((3,3),(0.14973948338295,0.97160236658079),
 .UNSPECIFIED.)
CURVE()
GEOMETRIC_REPRESENTATION_ITEM()
RATIONAL_B_SPLINE_CURVE((1.07140024848292,1.23714644374248,1.07140024848292))
REPRESENTATION_ITEM('')
);
#149=(
BOUNDED_CURVE()
B_SPLINE_CURVE(2,(#5244,#5245,#5246),.UNSPECIFIED.,.F.,.F.)
B_SPLINE_CURVE_WITH_KNOTS((3,3),(0.14973948338295,0.97160236658079),
 .UNSPECIFIED.)
CURVE()
GEOMETRIC_REPRESENTATION_ITEM()
RATIONAL_B_SPLINE_CURVE((1.07140024848292,1.23714644374248,1.07140024848292))
REPRESENTATION_ITEM('')
);
#150=(
BOUNDED_CURVE()
B_SPLINE_CURVE(2,(#5248,#5249,#5250),.UNSPECIFIED.,.F.,.F.)
B_SPLINE_CURVE_WITH_KNOTS((3,3),(0.14973948338295,0.971602366580789),
 .UNSPECIFIED.)
CURVE()
GEOMETRIC_REPRESENTATION_ITEM()
RATIONAL_B_SPLINE_CURVE((1.07140024848292,1.23714644374248,1.07140024848292))
REPRESENTATION_ITEM('')
);
#151=(
BOUNDED_CURVE()
B_SPLINE_CURVE(2,(#5255,#5256,#5257),.UNSPECIFIED.,.F.,.F.)
B_SPLINE_CURVE_WITH_KNOTS((3,3),(0.14973948338295,0.97160236658079),
 .UNSPECIFIED.)
CURVE()
GEOMETRIC_REPRESENTATION_ITEM()
RATIONAL_B_SPLINE_CURVE((1.07140024848292,1.23714644374248,1.07140024848292))
REPRESENTATION_ITEM('')
);
#152=(
BOUNDED_CURVE()
B_SPLINE_CURVE(2,(#5259,#5260,#5261),.UNSPECIFIED.,.F.,.F.)
B_SPLINE_CURVE_WITH_KNOTS((3,3),(0.14973948338295,0.97160236658079),
 .UNSPECIFIED.)
CURVE()
GEOMETRIC_REPRESENTATION_ITEM()
RATIONAL_B_SPLINE_CURVE((1.07140024848292,1.23714644374248,1.07140024848292))
REPRESENTATION_ITEM('')
);
#153=(
BOUNDED_CURVE()
B_SPLINE_CURVE(2,(#5263,#5264,#5265),.UNSPECIFIED.,.F.,.F.)
B_SPLINE_CURVE_WITH_KNOTS((3,3),(0.14973948338295,0.971602366580789),
 .UNSPECIFIED.)
CURVE()
GEOMETRIC_REPRESENTATION_ITEM()
RATIONAL_B_SPLINE_CURVE((1.07140024848292,1.23714644374248,1.07140024848292))
REPRESENTATION_ITEM('')
);
#154=(
BOUNDED_CURVE()
B_SPLINE_CURVE(2,(#5266,#5267,#5268),.UNSPECIFIED.,.F.,.F.)
B_SPLINE_CURVE_WITH_KNOTS((3,3),(0.14973948338295,0.97160236658079),
 .UNSPECIFIED.)
CURVE()
GEOMETRIC_REPRESENTATION_ITEM()
RATIONAL_B_SPLINE_CURVE((1.07140024848292,1.23714644374248,1.07140024848292))
REPRESENTATION_ITEM('')
);
#155=(
BOUNDED_CURVE()
B_SPLINE_CURVE(2,(#5275,#5276,#5277),.UNSPECIFIED.,.F.,.F.)
B_SPLINE_CURVE_WITH_KNOTS((3,3),(0.14973948338295,0.97160236658079),
 .UNSPECIFIED.)
CURVE()
GEOMETRIC_REPRESENTATION_ITEM()
RATIONAL_B_SPLINE_CURVE((1.07140024848292,1.23714644374248,1.07140024848292))
REPRESENTATION_ITEM('')
);
#156=(
BOUNDED_CURVE()
B_SPLINE_CURVE(2,(#5279,#5280,#5281),.UNSPECIFIED.,.F.,.F.)
B_SPLINE_CURVE_WITH_KNOTS((3,3),(0.14973948338295,0.97160236658079),
 .UNSPECIFIED.)
CURVE()
GEOMETRIC_REPRESENTATION_ITEM()
RATIONAL_B_SPLINE_CURVE((1.07140024848292,1.23714644374248,1.07140024848292))
REPRESENTATION_ITEM('')
);
#157=(
BOUNDED_CURVE()
B_SPLINE_CURVE(2,(#5283,#5284,#5285),.UNSPECIFIED.,.F.,.F.)
B_SPLINE_CURVE_WITH_KNOTS((3,3),(0.14973948338295,0.971602366580789),
 .UNSPECIFIED.)
CURVE()
GEOMETRIC_REPRESENTATION_ITEM()
RATIONAL_B_SPLINE_CURVE((1.07140024848292,1.23714644374248,1.07140024848292))
REPRESENTATION_ITEM('')
);
#158=(
BOUNDED_CURVE()
B_SPLINE_CURVE(2,(#5287,#5288,#5289),.UNSPECIFIED.,.F.,.F.)
B_SPLINE_CURVE_WITH_KNOTS((3,3),(0.14973948338295,0.97160236658079),
 .UNSPECIFIED.)
CURVE()
GEOMETRIC_REPRESENTATION_ITEM()
RATIONAL_B_SPLINE_CURVE((1.07140024848292,1.23714644374248,1.07140024848292))
REPRESENTATION_ITEM('')
);
#159=(
BOUNDED_CURVE()
B_SPLINE_CURVE(2,(#5291,#5292,#5293),.UNSPECIFIED.,.F.,.F.)
B_SPLINE_CURVE_WITH_KNOTS((3,3),(0.14973948338295,0.97160236658079),
 .UNSPECIFIED.)
CURVE()
GEOMETRIC_REPRESENTATION_ITEM()
RATIONAL_B_SPLINE_CURVE((1.07140024848292,1.23714644374248,1.07140024848292))
REPRESENTATION_ITEM('')
);
#160=(
BOUNDED_CURVE()
B_SPLINE_CURVE(2,(#5294,#5295,#5296),.UNSPECIFIED.,.F.,.F.)
B_SPLINE_CURVE_WITH_KNOTS((3,3),(0.14973948338295,0.971602366580789),
 .UNSPECIFIED.)
CURVE()
GEOMETRIC_REPRESENTATION_ITEM()
RATIONAL_B_SPLINE_CURVE((1.07140024848292,1.23714644374248,1.07140024848292))
REPRESENTATION_ITEM('')
);
#161=ORIENTED_CLOSED_SHELL('',*,#3175,.F.);
#162=BREP_WITH_VOIDS('Body1',#3176,(#161));
#163=CONICAL_SURFACE('',#3399,0.275,0.785398163397449);
#164=CONICAL_SURFACE('',#3422,0.4,0.785398163397448);
#165=CONICAL_SURFACE('',#3426,0.41,0.785398163397448);
#166=CONICAL_SURFACE('',#3430,0.26,0.463647609000806);
#167=CONICAL_SURFACE('',#3456,0.36,0.785398163397451);
#168=CONICAL_SURFACE('',#3459,0.734027674973257,1.0471975511966);
#169=CONICAL_SURFACE('',#3517,0.734027674973257,1.0471975511966);
#170=CONICAL_SURFACE('',#3519,0.734027674973257,1.0471975511966);
#171=ELLIPSE('',#3388,0.299389011154384,0.2117);
#172=ELLIPSE('',#3392,0.299389011154384,0.2117);
#173=SHAPE_REPRESENTATION_RELATIONSHIP('SRR','None',#5564,#184);
#174=SHAPE_REPRESENTATION_RELATIONSHIP('SRR','None',#5565,#185);
#175=SHAPE_REPRESENTATION_RELATIONSHIP('SRR','None',#5566,#186);
#176=SHAPE_REPRESENTATION_RELATIONSHIP('SRR','None',#5567,#187);
#177=SHAPE_REPRESENTATION_RELATIONSHIP('SRR','None',#5568,#188);
#178=SHAPE_REPRESENTATION_RELATIONSHIP('SRR','None',#5571,#189);
#179=SHAPE_REPRESENTATION_RELATIONSHIP('SRR','None',#5572,#190);
#180=SHAPE_REPRESENTATION_RELATIONSHIP('SRR','None',#5574,#191);
#181=SHAPE_REPRESENTATION_RELATIONSHIP('SRR','None',#5575,#192);
#182=SHAPE_REPRESENTATION_RELATIONSHIP('SRR','None',#5576,#193);
#183=SHAPE_REPRESENTATION_RELATIONSHIP('SRR','None',#5577,#194);
#184=ADVANCED_BREP_SHAPE_REPRESENTATION('',(#206),#5478);
#185=ADVANCED_BREP_SHAPE_REPRESENTATION('',(#207),#5479);
#186=ADVANCED_BREP_SHAPE_REPRESENTATION('',(#208),#5480);
#187=ADVANCED_BREP_SHAPE_REPRESENTATION('',(#209),#5481);
#188=ADVANCED_BREP_SHAPE_REPRESENTATION('',(#162),#5482);
#189=ADVANCED_BREP_SHAPE_REPRESENTATION('',(#210),#5485);
#190=ADVANCED_BREP_SHAPE_REPRESENTATION('',(#211),#5486);
#191=ADVANCED_BREP_SHAPE_REPRESENTATION('',(#212),#5488);
#192=ADVANCED_BREP_SHAPE_REPRESENTATION('',(#213),#5489);
#193=ADVANCED_BREP_SHAPE_REPRESENTATION('',(#214),#5490);
#194=ADVANCED_BREP_SHAPE_REPRESENTATION('',(#215),#5491);
#195=STYLED_ITEM('',(#5680),#206);
#196=STYLED_ITEM('',(#5715),#207);
#197=STYLED_ITEM('',(#5708),#208);
#198=STYLED_ITEM('',(#5708),#209);
#199=STYLED_ITEM('',(#5708),#162);
#200=STYLED_ITEM('',(#5687),#210);
#201=STYLED_ITEM('',(#5708),#211);
#202=STYLED_ITEM('',(#5694),#212);
#203=STYLED_ITEM('',(#5708),#213);
#204=STYLED_ITEM('',(#5708),#214);
#205=STYLED_ITEM('',(#5708),#215);
#206=MANIFOLD_SOLID_BREP('Body1',#3171);
#207=MANIFOLD_SOLID_BREP('Body1',#3172);
#208=MANIFOLD_SOLID_BREP('Body1',#3173);
#209=MANIFOLD_SOLID_BREP('Body1',#3174);
#210=MANIFOLD_SOLID_BREP('Body1',#3177);
#211=MANIFOLD_SOLID_BREP('Body1',#3178);
#212=MANIFOLD_SOLID_BREP('Body1',#3179);
#213=MANIFOLD_SOLID_BREP('Body1',#3180);
#214=MANIFOLD_SOLID_BREP('Body1',#3181);
#215=MANIFOLD_SOLID_BREP('Body1',#3182);
#216=FACE_BOUND('',#547,.T.);
#217=FACE_BOUND('',#549,.T.);
#218=FACE_BOUND('',#550,.T.);
#219=FACE_BOUND('',#552,.T.);
#220=FACE_BOUND('',#557,.T.);
#221=FACE_BOUND('',#558,.T.);
#222=FACE_BOUND('',#605,.T.);
#223=FACE_BOUND('',#607,.T.);
#224=FACE_BOUND('',#611,.T.);
#225=FACE_BOUND('',#626,.T.);
#226=FACE_BOUND('',#629,.T.);
#227=FACE_BOUND('',#644,.T.);
#228=FACE_BOUND('',#652,.T.);
#229=FACE_BOUND('',#653,.T.);
#230=FACE_BOUND('',#657,.T.);
#231=FACE_BOUND('',#658,.T.);
#232=FACE_BOUND('',#671,.T.);
#233=FACE_BOUND('',#684,.T.);
#234=FACE_BOUND('',#685,.T.);
#235=FACE_BOUND('',#686,.T.);
#236=FACE_BOUND('',#687,.T.);
#237=FACE_BOUND('',#688,.T.);
#238=FACE_BOUND('',#692,.T.);
#239=FACE_BOUND('',#693,.T.);
#240=FACE_BOUND('',#694,.T.);
#241=FACE_BOUND('',#695,.T.);
#242=FACE_BOUND('',#696,.T.);
#243=FACE_BOUND('',#700,.T.);
#244=FACE_BOUND('',#702,.T.);
#245=FACE_BOUND('',#713,.T.);
#246=FACE_BOUND('',#715,.T.);
#247=FACE_BOUND('',#723,.T.);
#248=FACE_BOUND('',#737,.T.);
#249=FACE_BOUND('',#740,.T.);
#250=PLANE('',#3317);
#251=PLANE('',#3318);
#252=PLANE('',#3319);
#253=PLANE('',#3320);
#254=PLANE('',#3321);
#255=PLANE('',#3322);
#256=PLANE('',#3323);
#257=PLANE('',#3324);
#258=PLANE('',#3325);
#259=PLANE('',#3326);
#260=PLANE('',#3328);
#261=PLANE('',#3329);
#262=PLANE('',#3330);
#263=PLANE('',#3331);
#264=PLANE('',#3332);
#265=PLANE('',#3333);
#266=PLANE('',#3334);
#267=PLANE('',#3335);
#268=PLANE('',#3336);
#269=PLANE('',#3337);
#270=PLANE('',#3338);
#271=PLANE('',#3339);
#272=PLANE('',#3340);
#273=PLANE('',#3341);
#274=PLANE('',#3342);
#275=PLANE('',#3343);
#276=PLANE('',#3344);
#277=PLANE('',#3345);
#278=PLANE('',#3346);
#279=PLANE('',#3347);
#280=PLANE('',#3348);
#281=PLANE('',#3349);
#282=PLANE('',#3350);
#283=PLANE('',#3351);
#284=PLANE('',#3352);
#285=PLANE('',#3353);
#286=PLANE('',#3354);
#287=PLANE('',#3355);
#288=PLANE('',#3356);
#289=PLANE('',#3357);
#290=PLANE('',#3358);
#291=PLANE('',#3359);
#292=PLANE('',#3360);
#293=PLANE('',#3361);
#294=PLANE('',#3362);
#295=PLANE('',#3363);
#296=PLANE('',#3367);
#297=PLANE('',#3368);
#298=PLANE('',#3369);
#299=PLANE('',#3370);
#300=PLANE('',#3371);
#301=PLANE('',#3372);
#302=PLANE('',#3373);
#303=PLANE('',#3374);
#304=PLANE('',#3375);
#305=PLANE('',#3376);
#306=PLANE('',#3378);
#307=PLANE('',#3379);
#308=PLANE('',#3380);
#309=PLANE('',#3382);
#310=PLANE('',#3383);
#311=PLANE('',#3384);
#312=PLANE('',#3385);
#313=PLANE('',#3386);
#314=PLANE('',#3387);
#315=PLANE('',#3394);
#316=PLANE('',#3395);
#317=PLANE('',#3396);
#318=PLANE('',#3397);
#319=PLANE('',#3404);
#320=PLANE('',#3408);
#321=PLANE('',#3410);
#322=PLANE('',#3411);
#323=PLANE('',#3412);
#324=PLANE('',#3413);
#325=PLANE('',#3414);
#326=PLANE('',#3415);
#327=PLANE('',#3416);
#328=PLANE('',#3417);
#329=PLANE('',#3418);
#330=PLANE('',#3420);
#331=PLANE('',#3428);
#332=PLANE('',#3445);
#333=PLANE('',#3446);
#334=PLANE('',#3448);
#335=PLANE('',#3451);
#336=PLANE('',#3458);
#337=PLANE('',#3461);
#338=PLANE('',#3462);
#339=PLANE('',#3463);
#340=PLANE('',#3464);
#341=PLANE('',#3465);
#342=PLANE('',#3466);
#343=PLANE('',#3467);
#344=PLANE('',#3468);
#345=PLANE('',#3495);
#346=PLANE('',#3496);
#347=PLANE('',#3497);
#348=PLANE('',#3498);
#349=PLANE('',#3499);
#350=PLANE('',#3500);
#351=PLANE('',#3501);
#352=PLANE('',#3503);
#353=PLANE('',#3506);
#354=PLANE('',#3514);
#355=PLANE('',#3515);
#356=PLANE('',#3521);
#357=PLANE('',#3522);
#358=PLANE('',#3523);
#359=PLANE('',#3527);
#360=PLANE('',#3528);
#361=PLANE('',#3529);
#362=PLANE('',#3530);
#363=PLANE('',#3531);
#364=PLANE('',#3551);
#365=PLANE('',#3571);
#366=PLANE('',#3572);
#367=PLANE('',#3573);
#368=PLANE('',#3574);
#369=PLANE('',#3575);
#370=PLANE('',#3576);
#371=PLANE('',#3577);
#372=PLANE('',#3580);
#373=FACE_OUTER_BOUND('',#540,.T.);
#374=FACE_OUTER_BOUND('',#541,.T.);
#375=FACE_OUTER_BOUND('',#542,.T.);
#376=FACE_OUTER_BOUND('',#543,.T.);
#377=FACE_OUTER_BOUND('',#544,.T.);
#378=FACE_OUTER_BOUND('',#545,.T.);
#379=FACE_OUTER_BOUND('',#546,.T.);
#380=FACE_OUTER_BOUND('',#548,.T.);
#381=FACE_OUTER_BOUND('',#551,.T.);
#382=FACE_OUTER_BOUND('',#553,.T.);
#383=FACE_OUTER_BOUND('',#554,.T.);
#384=FACE_OUTER_BOUND('',#555,.T.);
#385=FACE_OUTER_BOUND('',#556,.T.);
#386=FACE_OUTER_BOUND('',#559,.T.);
#387=FACE_OUTER_BOUND('',#560,.T.);
#388=FACE_OUTER_BOUND('',#561,.T.);
#389=FACE_OUTER_BOUND('',#562,.T.);
#390=FACE_OUTER_BOUND('',#563,.T.);
#391=FACE_OUTER_BOUND('',#564,.T.);
#392=FACE_OUTER_BOUND('',#565,.T.);
#393=FACE_OUTER_BOUND('',#566,.T.);
#394=FACE_OUTER_BOUND('',#567,.T.);
#395=FACE_OUTER_BOUND('',#568,.T.);
#396=FACE_OUTER_BOUND('',#569,.T.);
#397=FACE_OUTER_BOUND('',#570,.T.);
#398=FACE_OUTER_BOUND('',#571,.T.);
#399=FACE_OUTER_BOUND('',#572,.T.);
#400=FACE_OUTER_BOUND('',#573,.T.);
#401=FACE_OUTER_BOUND('',#574,.T.);
#402=FACE_OUTER_BOUND('',#575,.T.);
#403=FACE_OUTER_BOUND('',#576,.T.);
#404=FACE_OUTER_BOUND('',#577,.T.);
#405=FACE_OUTER_BOUND('',#578,.T.);
#406=FACE_OUTER_BOUND('',#579,.T.);
#407=FACE_OUTER_BOUND('',#580,.T.);
#408=FACE_OUTER_BOUND('',#581,.T.);
#409=FACE_OUTER_BOUND('',#582,.T.);
#410=FACE_OUTER_BOUND('',#583,.T.);
#411=FACE_OUTER_BOUND('',#584,.T.);
#412=FACE_OUTER_BOUND('',#585,.T.);
#413=FACE_OUTER_BOUND('',#586,.T.);
#414=FACE_OUTER_BOUND('',#587,.T.);
#415=FACE_OUTER_BOUND('',#588,.T.);
#416=FACE_OUTER_BOUND('',#589,.T.);
#417=FACE_OUTER_BOUND('',#590,.T.);
#418=FACE_OUTER_BOUND('',#591,.T.);
#419=FACE_OUTER_BOUND('',#592,.T.);
#420=FACE_OUTER_BOUND('',#593,.T.);
#421=FACE_OUTER_BOUND('',#594,.T.);
#422=FACE_OUTER_BOUND('',#595,.T.);
#423=FACE_OUTER_BOUND('',#596,.T.);
#424=FACE_OUTER_BOUND('',#597,.T.);
#425=FACE_OUTER_BOUND('',#598,.T.);
#426=FACE_OUTER_BOUND('',#599,.T.);
#427=FACE_OUTER_BOUND('',#600,.T.);
#428=FACE_OUTER_BOUND('',#601,.T.);
#429=FACE_OUTER_BOUND('',#602,.T.);
#430=FACE_OUTER_BOUND('',#603,.T.);
#431=FACE_OUTER_BOUND('',#604,.T.);
#432=FACE_OUTER_BOUND('',#606,.T.);
#433=FACE_OUTER_BOUND('',#608,.T.);
#434=FACE_OUTER_BOUND('',#609,.T.);
#435=FACE_OUTER_BOUND('',#610,.T.);
#436=FACE_OUTER_BOUND('',#612,.T.);
#437=FACE_OUTER_BOUND('',#613,.T.);
#438=FACE_OUTER_BOUND('',#614,.T.);
#439=FACE_OUTER_BOUND('',#615,.T.);
#440=FACE_OUTER_BOUND('',#616,.T.);
#441=FACE_OUTER_BOUND('',#617,.T.);
#442=FACE_OUTER_BOUND('',#618,.T.);
#443=FACE_OUTER_BOUND('',#619,.T.);
#444=FACE_OUTER_BOUND('',#620,.T.);
#445=FACE_OUTER_BOUND('',#621,.T.);
#446=FACE_OUTER_BOUND('',#622,.T.);
#447=FACE_OUTER_BOUND('',#623,.T.);
#448=FACE_OUTER_BOUND('',#624,.T.);
#449=FACE_OUTER_BOUND('',#625,.T.);
#450=FACE_OUTER_BOUND('',#627,.T.);
#451=FACE_OUTER_BOUND('',#628,.T.);
#452=FACE_OUTER_BOUND('',#630,.T.);
#453=FACE_OUTER_BOUND('',#631,.T.);
#454=FACE_OUTER_BOUND('',#632,.T.);
#455=FACE_OUTER_BOUND('',#633,.T.);
#456=FACE_OUTER_BOUND('',#634,.T.);
#457=FACE_OUTER_BOUND('',#635,.T.);
#458=FACE_OUTER_BOUND('',#636,.T.);
#459=FACE_OUTER_BOUND('',#637,.T.);
#460=FACE_OUTER_BOUND('',#638,.T.);
#461=FACE_OUTER_BOUND('',#639,.T.);
#462=FACE_OUTER_BOUND('',#640,.T.);
#463=FACE_OUTER_BOUND('',#641,.T.);
#464=FACE_OUTER_BOUND('',#642,.T.);
#465=FACE_OUTER_BOUND('',#643,.T.);
#466=FACE_OUTER_BOUND('',#645,.T.);
#467=FACE_OUTER_BOUND('',#646,.T.);
#468=FACE_OUTER_BOUND('',#647,.T.);
#469=FACE_OUTER_BOUND('',#648,.T.);
#470=FACE_OUTER_BOUND('',#649,.T.);
#471=FACE_OUTER_BOUND('',#650,.T.);
#472=FACE_OUTER_BOUND('',#651,.T.);
#473=FACE_OUTER_BOUND('',#654,.T.);
#474=FACE_OUTER_BOUND('',#655,.T.);
#475=FACE_OUTER_BOUND('',#656,.T.);
#476=FACE_OUTER_BOUND('',#659,.T.);
#477=FACE_OUTER_BOUND('',#660,.T.);
#478=FACE_OUTER_BOUND('',#661,.T.);
#479=FACE_OUTER_BOUND('',#662,.T.);
#480=FACE_OUTER_BOUND('',#663,.T.);
#481=FACE_OUTER_BOUND('',#664,.T.);
#482=FACE_OUTER_BOUND('',#665,.T.);
#483=FACE_OUTER_BOUND('',#666,.T.);
#484=FACE_OUTER_BOUND('',#667,.T.);
#485=FACE_OUTER_BOUND('',#668,.T.);
#486=FACE_OUTER_BOUND('',#669,.T.);
#487=FACE_OUTER_BOUND('',#670,.T.);
#488=FACE_OUTER_BOUND('',#672,.T.);
#489=FACE_OUTER_BOUND('',#673,.T.);
#490=FACE_OUTER_BOUND('',#674,.T.);
#491=FACE_OUTER_BOUND('',#675,.T.);
#492=FACE_OUTER_BOUND('',#676,.T.);
#493=FACE_OUTER_BOUND('',#677,.T.);
#494=FACE_OUTER_BOUND('',#678,.T.);
#495=FACE_OUTER_BOUND('',#679,.T.);
#496=FACE_OUTER_BOUND('',#680,.T.);
#497=FACE_OUTER_BOUND('',#681,.T.);
#498=FACE_OUTER_BOUND('',#682,.T.);
#499=FACE_OUTER_BOUND('',#683,.T.);
#500=FACE_OUTER_BOUND('',#689,.T.);
#501=FACE_OUTER_BOUND('',#690,.T.);
#502=FACE_OUTER_BOUND('',#691,.T.);
#503=FACE_OUTER_BOUND('',#697,.T.);
#504=FACE_OUTER_BOUND('',#698,.T.);
#505=FACE_OUTER_BOUND('',#699,.T.);
#506=FACE_OUTER_BOUND('',#701,.T.);
#507=FACE_OUTER_BOUND('',#703,.T.);
#508=FACE_OUTER_BOUND('',#704,.T.);
#509=FACE_OUTER_BOUND('',#705,.T.);
#510=FACE_OUTER_BOUND('',#706,.T.);
#511=FACE_OUTER_BOUND('',#707,.T.);
#512=FACE_OUTER_BOUND('',#708,.T.);
#513=FACE_OUTER_BOUND('',#709,.T.);
#514=FACE_OUTER_BOUND('',#710,.T.);
#515=FACE_OUTER_BOUND('',#711,.T.);
#516=FACE_OUTER_BOUND('',#712,.T.);
#517=FACE_OUTER_BOUND('',#714,.T.);
#518=FACE_OUTER_BOUND('',#716,.T.);
#519=FACE_OUTER_BOUND('',#717,.T.);
#520=FACE_OUTER_BOUND('',#718,.T.);
#521=FACE_OUTER_BOUND('',#719,.T.);
#522=FACE_OUTER_BOUND('',#720,.T.);
#523=FACE_OUTER_BOUND('',#721,.T.);
#524=FACE_OUTER_BOUND('',#722,.T.);
#525=FACE_OUTER_BOUND('',#724,.T.);
#526=FACE_OUTER_BOUND('',#725,.T.);
#527=FACE_OUTER_BOUND('',#726,.T.);
#528=FACE_OUTER_BOUND('',#727,.T.);
#529=FACE_OUTER_BOUND('',#728,.T.);
#530=FACE_OUTER_BOUND('',#729,.T.);
#531=FACE_OUTER_BOUND('',#730,.T.);
#532=FACE_OUTER_BOUND('',#731,.T.);
#533=FACE_OUTER_BOUND('',#732,.T.);
#534=FACE_OUTER_BOUND('',#733,.T.);
#535=FACE_OUTER_BOUND('',#734,.T.);
#536=FACE_OUTER_BOUND('',#735,.T.);
#537=FACE_OUTER_BOUND('',#736,.T.);
#538=FACE_OUTER_BOUND('',#738,.T.);
#539=FACE_OUTER_BOUND('',#739,.T.);
#540=EDGE_LOOP('',(#2138,#2139,#2140,#2141));
#541=EDGE_LOOP('',(#2142,#2143,#2144,#2145));
#542=EDGE_LOOP('',(#2146,#2147,#2148,#2149));
#543=EDGE_LOOP('',(#2150,#2151,#2152,#2153));
#544=EDGE_LOOP('',(#2154,#2155,#2156,#2157));
#545=EDGE_LOOP('',(#2158,#2159,#2160,#2161));
#546=EDGE_LOOP('',(#2162,#2163,#2164,#2165));
#547=EDGE_LOOP('',(#2166));
#548=EDGE_LOOP('',(#2167,#2168,#2169,#2170,#2171,#2172,#2173,#2174));
#549=EDGE_LOOP('',(#2175));
#550=EDGE_LOOP('',(#2176));
#551=EDGE_LOOP('',(#2177,#2178,#2179,#2180,#2181,#2182,#2183,#2184));
#552=EDGE_LOOP('',(#2185));
#553=EDGE_LOOP('',(#2186,#2187,#2188,#2189));
#554=EDGE_LOOP('',(#2190,#2191,#2192,#2193));
#555=EDGE_LOOP('',(#2194,#2195,#2196,#2197));
#556=EDGE_LOOP('',(#2198,#2199,#2200,#2201));
#557=EDGE_LOOP('',(#2202));
#558=EDGE_LOOP('',(#2203));
#559=EDGE_LOOP('',(#2204,#2205,#2206,#2207));
#560=EDGE_LOOP('',(#2208,#2209,#2210,#2211));
#561=EDGE_LOOP('',(#2212,#2213,#2214,#2215));
#562=EDGE_LOOP('',(#2216,#2217,#2218,#2219));
#563=EDGE_LOOP('',(#2220,#2221,#2222,#2223));
#564=EDGE_LOOP('',(#2224,#2225,#2226,#2227));
#565=EDGE_LOOP('',(#2228,#2229,#2230,#2231));
#566=EDGE_LOOP('',(#2232,#2233,#2234,#2235));
#567=EDGE_LOOP('',(#2236,#2237,#2238,#2239));
#568=EDGE_LOOP('',(#2240,#2241,#2242,#2243));
#569=EDGE_LOOP('',(#2244,#2245,#2246,#2247));
#570=EDGE_LOOP('',(#2248,#2249,#2250,#2251));
#571=EDGE_LOOP('',(#2252,#2253,#2254,#2255));
#572=EDGE_LOOP('',(#2256,#2257,#2258,#2259));
#573=EDGE_LOOP('',(#2260,#2261,#2262,#2263));
#574=EDGE_LOOP('',(#2264,#2265,#2266,#2267));
#575=EDGE_LOOP('',(#2268,#2269,#2270,#2271));
#576=EDGE_LOOP('',(#2272,#2273,#2274,#2275));
#577=EDGE_LOOP('',(#2276,#2277,#2278,#2279));
#578=EDGE_LOOP('',(#2280,#2281,#2282,#2283));
#579=EDGE_LOOP('',(#2284,#2285,#2286,#2287));
#580=EDGE_LOOP('',(#2288,#2289,#2290,#2291));
#581=EDGE_LOOP('',(#2292,#2293,#2294,#2295));
#582=EDGE_LOOP('',(#2296,#2297,#2298,#2299));
#583=EDGE_LOOP('',(#2300,#2301,#2302,#2303));
#584=EDGE_LOOP('',(#2304,#2305,#2306,#2307));
#585=EDGE_LOOP('',(#2308,#2309,#2310,#2311));
#586=EDGE_LOOP('',(#2312,#2313,#2314,#2315));
#587=EDGE_LOOP('',(#2316,#2317,#2318,#2319));
#588=EDGE_LOOP('',(#2320,#2321,#2322,#2323));
#589=EDGE_LOOP('',(#2324,#2325,#2326,#2327));
#590=EDGE_LOOP('',(#2328,#2329,#2330,#2331));
#591=EDGE_LOOP('',(#2332,#2333,#2334,#2335));
#592=EDGE_LOOP('',(#2336,#2337,#2338,#2339));
#593=EDGE_LOOP('',(#2340,#2341,#2342,#2343));
#594=EDGE_LOOP('',(#2344,#2345,#2346,#2347));
#595=EDGE_LOOP('',(#2348,#2349,#2350,#2351));
#596=EDGE_LOOP('',(#2352,#2353,#2354,#2355));
#597=EDGE_LOOP('',(#2356,#2357,#2358,#2359));
#598=EDGE_LOOP('',(#2360,#2361,#2362,#2363));
#599=EDGE_LOOP('',(#2364,#2365,#2366,#2367));
#600=EDGE_LOOP('',(#2368,#2369,#2370,#2371));
#601=EDGE_LOOP('',(#2372,#2373,#2374,#2375));
#602=EDGE_LOOP('',(#2376,#2377,#2378,#2379));
#603=EDGE_LOOP('',(#2380,#2381,#2382,#2383));
#604=EDGE_LOOP('',(#2384,#2385,#2386,#2387,#2388,#2389,#2390,#2391,#2392,
#2393,#2394,#2395,#2396,#2397,#2398,#2399,#2400,#2401,#2402,#2403,#2404,
#2405,#2406,#2407,#2408,#2409,#2410,#2411,#2412,#2413,#2414,#2415,#2416,
#2417,#2418,#2419,#2420,#2421,#2422,#2423,#2424,#2425,#2426,#2427));
#605=EDGE_LOOP('',(#2428));
#606=EDGE_LOOP('',(#2429,#2430,#2431,#2432,#2433,#2434,#2435,#2436,#2437,
#2438,#2439,#2440,#2441,#2442,#2443,#2444,#2445,#2446,#2447,#2448,#2449,
#2450,#2451,#2452,#2453,#2454,#2455,#2456,#2457,#2458,#2459,#2460,#2461,
#2462,#2463,#2464,#2465,#2466,#2467,#2468,#2469,#2470,#2471,#2472));
#607=EDGE_LOOP('',(#2473));
#608=EDGE_LOOP('',(#2474,#2475,#2476,#2477));
#609=EDGE_LOOP('',(#2478,#2479,#2480,#2481));
#610=EDGE_LOOP('',(#2482,#2483,#2484,#2485));
#611=EDGE_LOOP('',(#2486));
#612=EDGE_LOOP('',(#2487,#2488,#2489,#2490,#2491,#2492,#2493,#2494,#2495,
#2496));
#613=EDGE_LOOP('',(#2497,#2498,#2499,#2500));
#614=EDGE_LOOP('',(#2501,#2502,#2503,#2504));
#615=EDGE_LOOP('',(#2505,#2506,#2507,#2508,#2509,#2510,#2511,#2512,#2513,
#2514));
#616=EDGE_LOOP('',(#2515,#2516,#2517,#2518));
#617=EDGE_LOOP('',(#2519,#2520,#2521,#2522,#2523,#2524));
#618=EDGE_LOOP('',(#2525,#2526,#2527,#2528,#2529,#2530,#2531,#2532));
#619=EDGE_LOOP('',(#2533,#2534,#2535,#2536,#2537));
#620=EDGE_LOOP('',(#2538,#2539,#2540,#2541));
#621=EDGE_LOOP('',(#2542,#2543,#2544,#2545,#2546,#2547));
#622=EDGE_LOOP('',(#2548,#2549,#2550,#2551));
#623=EDGE_LOOP('',(#2552,#2553,#2554,#2555));
#624=EDGE_LOOP('',(#2556,#2557,#2558,#2559));
#625=EDGE_LOOP('',(#2560));
#626=EDGE_LOOP('',(#2561));
#627=EDGE_LOOP('',(#2562,#2563,#2564,#2565));
#628=EDGE_LOOP('',(#2566));
#629=EDGE_LOOP('',(#2567));
#630=EDGE_LOOP('',(#2568,#2569,#2570,#2571));
#631=EDGE_LOOP('',(#2572,#2573,#2574,#2575));
#632=EDGE_LOOP('',(#2576,#2577,#2578,#2579));
#633=EDGE_LOOP('',(#2580,#2581,#2582,#2583));
#634=EDGE_LOOP('',(#2584,#2585,#2586,#2587));
#635=EDGE_LOOP('',(#2588,#2589,#2590,#2591));
#636=EDGE_LOOP('',(#2592,#2593,#2594,#2595,#2596,#2597));
#637=EDGE_LOOP('',(#2598,#2599,#2600,#2601,#2602,#2603));
#638=EDGE_LOOP('',(#2604));
#639=EDGE_LOOP('',(#2605));
#640=EDGE_LOOP('',(#2606,#2607,#2608,#2609));
#641=EDGE_LOOP('',(#2610,#2611,#2612,#2613));
#642=EDGE_LOOP('',(#2614,#2615,#2616,#2617));
#643=EDGE_LOOP('',(#2618));
#644=EDGE_LOOP('',(#2619));
#645=EDGE_LOOP('',(#2620,#2621,#2622,#2623));
#646=EDGE_LOOP('',(#2624,#2625,#2626,#2627));
#647=EDGE_LOOP('',(#2628,#2629,#2630,#2631));
#648=EDGE_LOOP('',(#2632,#2633,#2634,#2635));
#649=EDGE_LOOP('',(#2636,#2637,#2638,#2639));
#650=EDGE_LOOP('',(#2640,#2641,#2642,#2643));
#651=EDGE_LOOP('',(#2644,#2645,#2646,#2647));
#652=EDGE_LOOP('',(#2648));
#653=EDGE_LOOP('',(#2649));
#654=EDGE_LOOP('',(#2650,#2651,#2652,#2653));
#655=EDGE_LOOP('',(#2654,#2655,#2656,#2657));
#656=EDGE_LOOP('',(#2658,#2659,#2660,#2661));
#657=EDGE_LOOP('',(#2662));
#658=EDGE_LOOP('',(#2663));
#659=EDGE_LOOP('',(#2664,#2665,#2666,#2667));
#660=EDGE_LOOP('',(#2668,#2669,#2670,#2671));
#661=EDGE_LOOP('',(#2672));
#662=EDGE_LOOP('',(#2673,#2674,#2675,#2676,#2677,#2678,#2679,#2680,#2681));
#663=EDGE_LOOP('',(#2682,#2683,#2684,#2685));
#664=EDGE_LOOP('',(#2686,#2687,#2688,#2689));
#665=EDGE_LOOP('',(#2690,#2691,#2692,#2693));
#666=EDGE_LOOP('',(#2694,#2695,#2696,#2697));
#667=EDGE_LOOP('',(#2698,#2699,#2700,#2701));
#668=EDGE_LOOP('',(#2702,#2703,#2704,#2705));
#669=EDGE_LOOP('',(#2706));
#670=EDGE_LOOP('',(#2707,#2708,#2709,#2710,#2711,#2712));
#671=EDGE_LOOP('',(#2713));
#672=EDGE_LOOP('',(#2714,#2715,#2716,#2717));
#673=EDGE_LOOP('',(#2718,#2719,#2720,#2721));
#674=EDGE_LOOP('',(#2722,#2723,#2724,#2725));
#675=EDGE_LOOP('',(#2726,#2727,#2728,#2729));
#676=EDGE_LOOP('',(#2730,#2731,#2732,#2733));
#677=EDGE_LOOP('',(#2734,#2735,#2736,#2737));
#678=EDGE_LOOP('',(#2738,#2739,#2740,#2741));
#679=EDGE_LOOP('',(#2742,#2743,#2744,#2745));
#680=EDGE_LOOP('',(#2746,#2747,#2748,#2749));
#681=EDGE_LOOP('',(#2750,#2751,#2752,#2753));
#682=EDGE_LOOP('',(#2754,#2755,#2756,#2757));
#683=EDGE_LOOP('',(#2758,#2759,#2760,#2761,#2762,#2763,#2764,#2765));
#684=EDGE_LOOP('',(#2766));
#685=EDGE_LOOP('',(#2767));
#686=EDGE_LOOP('',(#2768));
#687=EDGE_LOOP('',(#2769));
#688=EDGE_LOOP('',(#2770));
#689=EDGE_LOOP('',(#2771,#2772,#2773,#2774));
#690=EDGE_LOOP('',(#2775,#2776,#2777,#2778));
#691=EDGE_LOOP('',(#2779,#2780,#2781,#2782,#2783,#2784,#2785,#2786));
#692=EDGE_LOOP('',(#2787));
#693=EDGE_LOOP('',(#2788));
#694=EDGE_LOOP('',(#2789));
#695=EDGE_LOOP('',(#2790));
#696=EDGE_LOOP('',(#2791));
#697=EDGE_LOOP('',(#2792,#2793,#2794,#2795));
#698=EDGE_LOOP('',(#2796,#2797,#2798,#2799));
#699=EDGE_LOOP('',(#2800));
#700=EDGE_LOOP('',(#2801));
#701=EDGE_LOOP('',(#2802));
#702=EDGE_LOOP('',(#2803));
#703=EDGE_LOOP('',(#2804,#2805,#2806,#2807,#2808,#2809,#2810,#2811,#2812));
#704=EDGE_LOOP('',(#2813,#2814,#2815,#2816,#2817,#2818,#2819,#2820,#2821));
#705=EDGE_LOOP('',(#2822,#2823,#2824,#2825));
#706=EDGE_LOOP('',(#2826,#2827,#2828,#2829));
#707=EDGE_LOOP('',(#2830,#2831,#2832,#2833));
#708=EDGE_LOOP('',(#2834,#2835,#2836,#2837));
#709=EDGE_LOOP('',(#2838,#2839,#2840,#2841));
#710=EDGE_LOOP('',(#2842,#2843,#2844,#2845));
#711=EDGE_LOOP('',(#2846,#2847,#2848,#2849));
#712=EDGE_LOOP('',(#2850));
#713=EDGE_LOOP('',(#2851));
#714=EDGE_LOOP('',(#2852));
#715=EDGE_LOOP('',(#2853));
#716=EDGE_LOOP('',(#2854,#2855,#2856,#2857));
#717=EDGE_LOOP('',(#2858,#2859,#2860,#2861));
#718=EDGE_LOOP('',(#2862,#2863,#2864,#2865));
#719=EDGE_LOOP('',(#2866,#2867,#2868,#2869));
#720=EDGE_LOOP('',(#2870,#2871,#2872,#2873));
#721=EDGE_LOOP('',(#2874,#2875,#2876,#2877));
#722=EDGE_LOOP('',(#2878,#2879,#2880,#2881,#2882,#2883,#2884,#2885,#2886,
#2887,#2888,#2889));
#723=EDGE_LOOP('',(#2890));
#724=EDGE_LOOP('',(#2891,#2892,#2893,#2894));
#725=EDGE_LOOP('',(#2895,#2896,#2897,#2898));
#726=EDGE_LOOP('',(#2899,#2900,#2901,#2902));
#727=EDGE_LOOP('',(#2903,#2904,#2905,#2906));
#728=EDGE_LOOP('',(#2907,#2908,#2909,#2910));
#729=EDGE_LOOP('',(#2911,#2912,#2913,#2914));
#730=EDGE_LOOP('',(#2915,#2916,#2917,#2918));
#731=EDGE_LOOP('',(#2919,#2920,#2921,#2922));
#732=EDGE_LOOP('',(#2923,#2924,#2925,#2926));
#733=EDGE_LOOP('',(#2927,#2928,#2929,#2930));
#734=EDGE_LOOP('',(#2931,#2932,#2933,#2934));
#735=EDGE_LOOP('',(#2935,#2936,#2937,#2938));
#736=EDGE_LOOP('',(#2939,#2940,#2941,#2942,#2943,#2944));
#737=EDGE_LOOP('',(#2945));
#738=EDGE_LOOP('',(#2946,#2947,#2948,#2949));
#739=EDGE_LOOP('',(#2950,#2951,#2952,#2953,#2954,#2955,#2956,#2957,#2958,
#2959,#2960,#2961));
#740=EDGE_LOOP('',(#2962,#2963,#2964,#2965,#2966,#2967));
#741=LINE('',#4525,#1054);
#742=LINE('',#4531,#1055);
#743=LINE('',#4537,#1056);
#744=LINE('',#4542,#1057);
#745=LINE('',#4544,#1058);
#746=LINE('',#4546,#1059);
#747=LINE('',#4547,#1060);
#748=LINE('',#4551,#1061);
#749=LINE('',#4553,#1062);
#750=LINE('',#4555,#1063);
#751=LINE('',#4556,#1064);
#752=LINE('',#4558,#1065);
#753=LINE('',#4559,#1066);
#754=LINE('',#4561,#1067);
#755=LINE('',#4564,#1068);
#756=LINE('',#4566,#1069);
#757=LINE('',#4568,#1070);
#758=LINE('',#4570,#1071);
#759=LINE('',#4571,#1072);
#760=LINE('',#4575,#1073);
#761=LINE('',#4576,#1074);
#762=LINE('',#4577,#1075);
#763=LINE('',#4580,#1076);
#764=LINE('',#4581,#1077);
#765=LINE('',#4584,#1078);
#766=LINE('',#4585,#1079);
#767=LINE('',#4587,#1080);
#768=LINE('',#4593,#1081);
#769=LINE('',#4595,#1082);
#770=LINE('',#4597,#1083);
#771=LINE('',#4598,#1084);
#772=LINE('',#4601,#1085);
#773=LINE('',#4603,#1086);
#774=LINE('',#4604,#1087);
#775=LINE('',#4607,#1088);
#776=LINE('',#4609,#1089);
#777=LINE('',#4610,#1090);
#778=LINE('',#4613,#1091);
#779=LINE('',#4615,#1092);
#780=LINE('',#4616,#1093);
#781=LINE('',#4619,#1094);
#782=LINE('',#4621,#1095);
#783=LINE('',#4622,#1096);
#784=LINE('',#4625,#1097);
#785=LINE('',#4627,#1098);
#786=LINE('',#4628,#1099);
#787=LINE('',#4631,#1100);
#788=LINE('',#4633,#1101);
#789=LINE('',#4634,#1102);
#790=LINE('',#4637,#1103);
#791=LINE('',#4639,#1104);
#792=LINE('',#4640,#1105);
#793=LINE('',#4643,#1106);
#794=LINE('',#4645,#1107);
#795=LINE('',#4646,#1108);
#796=LINE('',#4650,#1109);
#797=LINE('',#4652,#1110);
#798=LINE('',#4654,#1111);
#799=LINE('',#4655,#1112);
#800=LINE('',#4658,#1113);
#801=LINE('',#4660,#1114);
#802=LINE('',#4661,#1115);
#803=LINE('',#4664,#1116);
#804=LINE('',#4666,#1117);
#805=LINE('',#4667,#1118);
#806=LINE('',#4670,#1119);
#807=LINE('',#4672,#1120);
#808=LINE('',#4673,#1121);
#809=LINE('',#4676,#1122);
#810=LINE('',#4678,#1123);
#811=LINE('',#4679,#1124);
#812=LINE('',#4682,#1125);
#813=LINE('',#4684,#1126);
#814=LINE('',#4685,#1127);
#815=LINE('',#4688,#1128);
#816=LINE('',#4690,#1129);
#817=LINE('',#4691,#1130);
#818=LINE('',#4694,#1131);
#819=LINE('',#4696,#1132);
#820=LINE('',#4697,#1133);
#821=LINE('',#4700,#1134);
#822=LINE('',#4702,#1135);
#823=LINE('',#4703,#1136);
#824=LINE('',#4707,#1137);
#825=LINE('',#4709,#1138);
#826=LINE('',#4711,#1139);
#827=LINE('',#4712,#1140);
#828=LINE('',#4715,#1141);
#829=LINE('',#4717,#1142);
#830=LINE('',#4718,#1143);
#831=LINE('',#4721,#1144);
#832=LINE('',#4723,#1145);
#833=LINE('',#4724,#1146);
#834=LINE('',#4727,#1147);
#835=LINE('',#4729,#1148);
#836=LINE('',#4730,#1149);
#837=LINE('',#4733,#1150);
#838=LINE('',#4735,#1151);
#839=LINE('',#4736,#1152);
#840=LINE('',#4739,#1153);
#841=LINE('',#4741,#1154);
#842=LINE('',#4742,#1155);
#843=LINE('',#4745,#1156);
#844=LINE('',#4747,#1157);
#845=LINE('',#4748,#1158);
#846=LINE('',#4751,#1159);
#847=LINE('',#4753,#1160);
#848=LINE('',#4754,#1161);
#849=LINE('',#4757,#1162);
#850=LINE('',#4759,#1163);
#851=LINE('',#4760,#1164);
#852=LINE('',#4764,#1165);
#853=LINE('',#4766,#1166);
#854=LINE('',#4768,#1167);
#855=LINE('',#4769,#1168);
#856=LINE('',#4772,#1169);
#857=LINE('',#4774,#1170);
#858=LINE('',#4775,#1171);
#859=LINE('',#4778,#1172);
#860=LINE('',#4780,#1173);
#861=LINE('',#4781,#1174);
#862=LINE('',#4784,#1175);
#863=LINE('',#4786,#1176);
#864=LINE('',#4787,#1177);
#865=LINE('',#4790,#1178);
#866=LINE('',#4792,#1179);
#867=LINE('',#4793,#1180);
#868=LINE('',#4796,#1181);
#869=LINE('',#4798,#1182);
#870=LINE('',#4799,#1183);
#871=LINE('',#4802,#1184);
#872=LINE('',#4804,#1185);
#873=LINE('',#4805,#1186);
#874=LINE('',#4808,#1187);
#875=LINE('',#4810,#1188);
#876=LINE('',#4811,#1189);
#877=LINE('',#4814,#1190);
#878=LINE('',#4816,#1191);
#879=LINE('',#4817,#1192);
#880=LINE('',#4822,#1193);
#881=LINE('',#4826,#1194);
#882=LINE('',#4828,#1195);
#883=LINE('',#4829,#1196);
#884=LINE('',#4832,#1197);
#885=LINE('',#4834,#1198);
#886=LINE('',#4835,#1199);
#887=LINE('',#4837,#1200);
#888=LINE('',#4838,#1201);
#889=LINE('',#4841,#1202);
#890=LINE('',#4843,#1203);
#891=LINE('',#4844,#1204);
#892=LINE('',#4846,#1205);
#893=LINE('',#4847,#1206);
#894=LINE('',#4850,#1207);
#895=LINE('',#4852,#1208);
#896=LINE('',#4853,#1209);
#897=LINE('',#4855,#1210);
#898=LINE('',#4856,#1211);
#899=LINE('',#4858,#1212);
#900=LINE('',#4859,#1213);
#901=LINE('',#4866,#1214);
#902=LINE('',#4868,#1215);
#903=LINE('',#4870,#1216);
#904=LINE('',#4871,#1217);
#905=LINE('',#4874,#1218);
#906=LINE('',#4876,#1219);
#907=LINE('',#4877,#1220);
#908=LINE('',#4880,#1221);
#909=LINE('',#4882,#1222);
#910=LINE('',#4883,#1223);
#911=LINE('',#4888,#1224);
#912=LINE('',#4890,#1225);
#913=LINE('',#4892,#1226);
#914=LINE('',#4894,#1227);
#915=LINE('',#4896,#1228);
#916=LINE('',#4898,#1229);
#917=LINE('',#4899,#1230);
#918=LINE('',#4902,#1231);
#919=LINE('',#4903,#1232);
#920=LINE('',#4906,#1233);
#921=LINE('',#4907,#1234);
#922=LINE('',#4910,#1235);
#923=LINE('',#4912,#1236);
#924=LINE('',#4914,#1237);
#925=LINE('',#4916,#1238);
#926=LINE('',#4917,#1239);
#927=LINE('',#4919,#1240);
#928=LINE('',#4922,#1241);
#929=LINE('',#4925,#1242);
#930=LINE('',#4929,#1243);
#931=LINE('',#4936,#1244);
#932=LINE('',#4938,#1245);
#933=LINE('',#4940,#1246);
#934=LINE('',#4947,#1247);
#935=LINE('',#4951,#1248);
#936=LINE('',#4958,#1249);
#937=LINE('',#4965,#1250);
#938=LINE('',#4967,#1251);
#939=LINE('',#4969,#1252);
#940=LINE('',#4970,#1253);
#941=LINE('',#4973,#1254);
#942=LINE('',#4975,#1255);
#943=LINE('',#4976,#1256);
#944=LINE('',#4979,#1257);
#945=LINE('',#4981,#1258);
#946=LINE('',#4982,#1259);
#947=LINE('',#4985,#1260);
#948=LINE('',#4987,#1261);
#949=LINE('',#4988,#1262);
#950=LINE('',#4991,#1263);
#951=LINE('',#4993,#1264);
#952=LINE('',#4994,#1265);
#953=LINE('',#4996,#1266);
#954=LINE('',#4997,#1267);
#955=LINE('',#5009,#1268);
#956=LINE('',#5013,#1269);
#957=LINE('',#5017,#1270);
#958=LINE('',#5024,#1271);
#959=LINE('',#5026,#1272);
#960=LINE('',#5034,#1273);
#961=LINE('',#5040,#1274);
#962=LINE('',#5045,#1275);
#963=LINE('',#5049,#1276);
#964=LINE('',#5053,#1277);
#965=LINE('',#5055,#1278);
#966=LINE('',#5056,#1279);
#967=LINE('',#5059,#1280);
#968=LINE('',#5063,#1281);
#969=LINE('',#5064,#1282);
#970=LINE('',#5073,#1283);
#971=LINE('',#5078,#1284);
#972=LINE('',#5084,#1285);
#973=LINE('',#5110,#1286);
#974=LINE('',#5112,#1287);
#975=LINE('',#5113,#1288);
#976=LINE('',#5116,#1289);
#977=LINE('',#5117,#1290);
#978=LINE('',#5120,#1291);
#979=LINE('',#5121,#1292);
#980=LINE('',#5124,#1293);
#981=LINE('',#5125,#1294);
#982=LINE('',#5128,#1295);
#983=LINE('',#5129,#1296);
#984=LINE('',#5131,#1297);
#985=LINE('',#5149,#1298);
#986=LINE('',#5155,#1299);
#987=LINE('',#5161,#1300);
#988=LINE('',#5167,#1301);
#989=LINE('',#5173,#1302);
#990=LINE('',#5178,#1303);
#991=LINE('',#5180,#1304);
#992=LINE('',#5182,#1305);
#993=LINE('',#5183,#1306);
#994=LINE('',#5187,#1307);
#995=LINE('',#5189,#1308);
#996=LINE('',#5191,#1309);
#997=LINE('',#5192,#1310);
#998=LINE('',#5196,#1311);
#999=LINE('',#5197,#1312);
#1000=LINE('',#5198,#1313);
#1001=LINE('',#5201,#1314);
#1002=LINE('',#5203,#1315);
#1003=LINE('',#5204,#1316);
#1004=LINE('',#5206,#1317);
#1005=LINE('',#5207,#1318);
#1006=LINE('',#5210,#1319);
#1007=LINE('',#5212,#1320);
#1008=LINE('',#5213,#1321);
#1009=LINE('',#5216,#1322);
#1010=LINE('',#5220,#1323);
#1011=LINE('',#5221,#1324);
#1012=LINE('',#5230,#1325);
#1013=LINE('',#5236,#1326);
#1014=LINE('',#5252,#1327);
#1015=LINE('',#5273,#1328);
#1016=LINE('',#5298,#1329);
#1017=LINE('',#5299,#1330);
#1018=LINE('',#5301,#1331);
#1019=LINE('',#5303,#1332);
#1020=LINE('',#5308,#1333);
#1021=LINE('',#5311,#1334);
#1022=LINE('',#5313,#1335);
#1023=LINE('',#5321,#1336);
#1024=LINE('',#5325,#1337);
#1025=LINE('',#5330,#1338);
#1026=LINE('',#5334,#1339);
#1027=LINE('',#5339,#1340);
#1028=LINE('',#5343,#1341);
#1029=LINE('',#5348,#1342);
#1030=LINE('',#5352,#1343);
#1031=LINE('',#5357,#1344);
#1032=LINE('',#5361,#1345);
#1033=LINE('',#5366,#1346);
#1034=LINE('',#5370,#1347);
#1035=LINE('',#5396,#1348);
#1036=LINE('',#5398,#1349);
#1037=LINE('',#5400,#1350);
#1038=LINE('',#5401,#1351);
#1039=LINE('',#5404,#1352);
#1040=LINE('',#5406,#1353);
#1041=LINE('',#5407,#1354);
#1042=LINE('',#5410,#1355);
#1043=LINE('',#5412,#1356);
#1044=LINE('',#5413,#1357);
#1045=LINE('',#5416,#1358);
#1046=LINE('',#5418,#1359);
#1047=LINE('',#5419,#1360);
#1048=LINE('',#5422,#1361);
#1049=LINE('',#5424,#1362);
#1050=LINE('',#5425,#1363);
#1051=LINE('',#5427,#1364);
#1052=LINE('',#5428,#1365);
#1053=LINE('',#5433,#1366);
#1054=VECTOR('',#3615,0.275);
#1055=VECTOR('',#3622,0.275);
#1056=VECTOR('',#3629,0.425);
#1057=VECTOR('',#3634,1.);
#1058=VECTOR('',#3635,1.);
#1059=VECTOR('',#3636,1.);
#1060=VECTOR('',#3637,1.);
#1061=VECTOR('',#3640,1.);
#1062=VECTOR('',#3641,1.);
#1063=VECTOR('',#3642,1.);
#1064=VECTOR('',#3643,1.);
#1065=VECTOR('',#3646,1.);
#1066=VECTOR('',#3647,1.);
#1067=VECTOR('',#3650,1.);
#1068=VECTOR('',#3653,1.);
#1069=VECTOR('',#3654,1.);
#1070=VECTOR('',#3655,1.);
#1071=VECTOR('',#3656,1.);
#1072=VECTOR('',#3657,1.);
#1073=VECTOR('',#3660,1.);
#1074=VECTOR('',#3661,1.);
#1075=VECTOR('',#3662,1.);
#1076=VECTOR('',#3665,1.);
#1077=VECTOR('',#3666,1.);
#1078=VECTOR('',#3669,1.);
#1079=VECTOR('',#3670,1.);
#1080=VECTOR('',#3673,1.);
#1081=VECTOR('',#3680,1.);
#1082=VECTOR('',#3681,1.);
#1083=VECTOR('',#3682,1.);
#1084=VECTOR('',#3683,1.);
#1085=VECTOR('',#3686,1.);
#1086=VECTOR('',#3687,1.);
#1087=VECTOR('',#3688,1.);
#1088=VECTOR('',#3691,1.);
#1089=VECTOR('',#3692,1.);
#1090=VECTOR('',#3693,1.);
#1091=VECTOR('',#3696,1.);
#1092=VECTOR('',#3697,1.);
#1093=VECTOR('',#3698,1.);
#1094=VECTOR('',#3701,1.);
#1095=VECTOR('',#3702,1.);
#1096=VECTOR('',#3703,1.);
#1097=VECTOR('',#3706,1.);
#1098=VECTOR('',#3707,1.);
#1099=VECTOR('',#3708,1.);
#1100=VECTOR('',#3711,1.);
#1101=VECTOR('',#3712,1.);
#1102=VECTOR('',#3713,1.);
#1103=VECTOR('',#3716,1.);
#1104=VECTOR('',#3717,1.);
#1105=VECTOR('',#3718,1.);
#1106=VECTOR('',#3721,1.);
#1107=VECTOR('',#3722,1.);
#1108=VECTOR('',#3723,1.);
#1109=VECTOR('',#3726,1.);
#1110=VECTOR('',#3727,1.);
#1111=VECTOR('',#3728,1.);
#1112=VECTOR('',#3729,1.);
#1113=VECTOR('',#3732,1.);
#1114=VECTOR('',#3733,1.);
#1115=VECTOR('',#3734,1.);
#1116=VECTOR('',#3737,1.);
#1117=VECTOR('',#3738,1.);
#1118=VECTOR('',#3739,1.);
#1119=VECTOR('',#3742,1.);
#1120=VECTOR('',#3743,1.);
#1121=VECTOR('',#3744,1.);
#1122=VECTOR('',#3747,1.);
#1123=VECTOR('',#3748,1.);
#1124=VECTOR('',#3749,1.);
#1125=VECTOR('',#3752,1.);
#1126=VECTOR('',#3753,1.);
#1127=VECTOR('',#3754,1.);
#1128=VECTOR('',#3757,1.);
#1129=VECTOR('',#3758,1.);
#1130=VECTOR('',#3759,1.);
#1131=VECTOR('',#3762,1.);
#1132=VECTOR('',#3763,1.);
#1133=VECTOR('',#3764,1.);
#1134=VECTOR('',#3767,1.);
#1135=VECTOR('',#3768,1.);
#1136=VECTOR('',#3769,1.);
#1137=VECTOR('',#3772,1.);
#1138=VECTOR('',#3773,1.);
#1139=VECTOR('',#3774,1.);
#1140=VECTOR('',#3775,1.);
#1141=VECTOR('',#3778,1.);
#1142=VECTOR('',#3779,1.);
#1143=VECTOR('',#3780,1.);
#1144=VECTOR('',#3783,1.);
#1145=VECTOR('',#3784,1.);
#1146=VECTOR('',#3785,1.);
#1147=VECTOR('',#3788,1.);
#1148=VECTOR('',#3789,1.);
#1149=VECTOR('',#3790,1.);
#1150=VECTOR('',#3793,1.);
#1151=VECTOR('',#3794,1.);
#1152=VECTOR('',#3795,1.);
#1153=VECTOR('',#3798,1.);
#1154=VECTOR('',#3799,1.);
#1155=VECTOR('',#3800,1.);
#1156=VECTOR('',#3803,1.);
#1157=VECTOR('',#3804,1.);
#1158=VECTOR('',#3805,1.);
#1159=VECTOR('',#3808,1.);
#1160=VECTOR('',#3809,1.);
#1161=VECTOR('',#3810,1.);
#1162=VECTOR('',#3813,1.);
#1163=VECTOR('',#3814,1.);
#1164=VECTOR('',#3815,1.);
#1165=VECTOR('',#3818,1.);
#1166=VECTOR('',#3819,1.);
#1167=VECTOR('',#3820,1.);
#1168=VECTOR('',#3821,1.);
#1169=VECTOR('',#3824,1.);
#1170=VECTOR('',#3825,1.);
#1171=VECTOR('',#3826,1.);
#1172=VECTOR('',#3829,1.);
#1173=VECTOR('',#3830,1.);
#1174=VECTOR('',#3831,1.);
#1175=VECTOR('',#3834,1.);
#1176=VECTOR('',#3835,1.);
#1177=VECTOR('',#3836,1.);
#1178=VECTOR('',#3839,1.);
#1179=VECTOR('',#3840,1.);
#1180=VECTOR('',#3841,1.);
#1181=VECTOR('',#3844,1.);
#1182=VECTOR('',#3845,1.);
#1183=VECTOR('',#3846,1.);
#1184=VECTOR('',#3849,1.);
#1185=VECTOR('',#3850,1.);
#1186=VECTOR('',#3851,1.);
#1187=VECTOR('',#3854,1.);
#1188=VECTOR('',#3855,1.);
#1189=VECTOR('',#3856,1.);
#1190=VECTOR('',#3859,1.);
#1191=VECTOR('',#3860,1.);
#1192=VECTOR('',#3861,1.);
#1193=VECTOR('',#3866,0.21);
#1194=VECTOR('',#3871,1.);
#1195=VECTOR('',#3872,1.);
#1196=VECTOR('',#3873,1.);
#1197=VECTOR('',#3876,1.);
#1198=VECTOR('',#3877,1.);
#1199=VECTOR('',#3878,1.);
#1200=VECTOR('',#3881,1.);
#1201=VECTOR('',#3882,1.);
#1202=VECTOR('',#3885,1.);
#1203=VECTOR('',#3886,1.);
#1204=VECTOR('',#3887,1.);
#1205=VECTOR('',#3890,1.);
#1206=VECTOR('',#3891,1.);
#1207=VECTOR('',#3894,1.);
#1208=VECTOR('',#3895,1.);
#1209=VECTOR('',#3896,1.);
#1210=VECTOR('',#3899,1.);
#1211=VECTOR('',#3900,1.);
#1212=VECTOR('',#3903,1.);
#1213=VECTOR('',#3904,1.);
#1214=VECTOR('',#3913,1.);
#1215=VECTOR('',#3914,1.);
#1216=VECTOR('',#3915,1.);
#1217=VECTOR('',#3916,1.);
#1218=VECTOR('',#3919,1.);
#1219=VECTOR('',#3920,1.);
#1220=VECTOR('',#3921,1.);
#1221=VECTOR('',#3924,1.);
#1222=VECTOR('',#3925,1.);
#1223=VECTOR('',#3926,1.);
#1224=VECTOR('',#3931,1.);
#1225=VECTOR('',#3932,1.);
#1226=VECTOR('',#3933,1.);
#1227=VECTOR('',#3934,1.);
#1228=VECTOR('',#3935,1.);
#1229=VECTOR('',#3936,1.);
#1230=VECTOR('',#3937,1.);
#1231=VECTOR('',#3940,1.);
#1232=VECTOR('',#3941,1.);
#1233=VECTOR('',#3944,1.);
#1234=VECTOR('',#3945,1.);
#1235=VECTOR('',#3948,1.);
#1236=VECTOR('',#3949,1.);
#1237=VECTOR('',#3950,1.);
#1238=VECTOR('',#3951,1.);
#1239=VECTOR('',#3952,1.);
#1240=VECTOR('',#3955,1.);
#1241=VECTOR('',#3958,1.);
#1242=VECTOR('',#3961,1.);
#1243=VECTOR('',#3966,0.21);
#1244=VECTOR('',#3975,1.);
#1245=VECTOR('',#3978,1.);
#1246=VECTOR('',#3981,1.);
#1247=VECTOR('',#3990,0.275);
#1248=VECTOR('',#3995,0.265);
#1249=VECTOR('',#4004,0.5);
#1250=VECTOR('',#4013,1.);
#1251=VECTOR('',#4014,1.);
#1252=VECTOR('',#4015,1.);
#1253=VECTOR('',#4016,1.);
#1254=VECTOR('',#4019,1.);
#1255=VECTOR('',#4020,1.);
#1256=VECTOR('',#4021,1.);
#1257=VECTOR('',#4024,1.);
#1258=VECTOR('',#4025,1.);
#1259=VECTOR('',#4026,1.);
#1260=VECTOR('',#4029,1.);
#1261=VECTOR('',#4030,1.);
#1262=VECTOR('',#4031,1.);
#1263=VECTOR('',#4034,1.);
#1264=VECTOR('',#4035,1.);
#1265=VECTOR('',#4036,1.);
#1266=VECTOR('',#4039,1.);
#1267=VECTOR('',#4040,1.);
#1268=VECTOR('',#4057,0.4);
#1269=VECTOR('',#4062,0.425);
#1270=VECTOR('',#4067,0.41);
#1271=VECTOR('',#4076,0.26);
#1272=VECTOR('',#4079,0.25);
#1273=VECTOR('',#4090,0.425);
#1274=VECTOR('',#4097,0.425000000000001);
#1275=VECTOR('',#4102,1.);
#1276=VECTOR('',#4105,1.);
#1277=VECTOR('',#4110,1.);
#1278=VECTOR('',#4111,1.);
#1279=VECTOR('',#4112,1.);
#1280=VECTOR('',#4115,1.);
#1281=VECTOR('',#4120,1.);
#1282=VECTOR('',#4121,1.);
#1283=VECTOR('',#4134,0.4);
#1284=VECTOR('',#4141,0.36);
#1285=VECTOR('',#4148,0.734027674973257);
#1286=VECTOR('',#4151,1.);
#1287=VECTOR('',#4152,1.);
#1288=VECTOR('',#4153,1.);
#1289=VECTOR('',#4156,1.);
#1290=VECTOR('',#4157,1.);
#1291=VECTOR('',#4160,1.);
#1292=VECTOR('',#4161,1.);
#1293=VECTOR('',#4164,1.);
#1294=VECTOR('',#4165,1.);
#1295=VECTOR('',#4168,1.);
#1296=VECTOR('',#4169,1.);
#1297=VECTOR('',#4172,1.);
#1298=VECTOR('',#4203,0.329999999999998);
#1299=VECTOR('',#4210,0.329999999999998);
#1300=VECTOR('',#4217,0.329999999999998);
#1301=VECTOR('',#4224,0.329999999999998);
#1302=VECTOR('',#4231,0.425000000000001);
#1303=VECTOR('',#4236,1.);
#1304=VECTOR('',#4237,1.);
#1305=VECTOR('',#4238,1.);
#1306=VECTOR('',#4239,1.);
#1307=VECTOR('',#4242,1.);
#1308=VECTOR('',#4243,1.);
#1309=VECTOR('',#4244,1.);
#1310=VECTOR('',#4245,1.);
#1311=VECTOR('',#4248,1.);
#1312=VECTOR('',#4249,1.);
#1313=VECTOR('',#4250,1.);
#1314=VECTOR('',#4253,1.);
#1315=VECTOR('',#4254,1.);
#1316=VECTOR('',#4255,1.);
#1317=VECTOR('',#4258,1.);
#1318=VECTOR('',#4259,1.);
#1319=VECTOR('',#4262,1.);
#1320=VECTOR('',#4263,1.);
#1321=VECTOR('',#4264,1.);
#1322=VECTOR('',#4267,1.);
#1323=VECTOR('',#4272,1.);
#1324=VECTOR('',#4273,1.);
#1325=VECTOR('',#4286,0.42);
#1326=VECTOR('',#4293,0.8);
#1327=VECTOR('',#4304,0.734027674973257);
#1328=VECTOR('',#4311,0.734027674973257);
#1329=VECTOR('',#4314,1.);
#1330=VECTOR('',#4315,1.);
#1331=VECTOR('',#4318,1.);
#1332=VECTOR('',#4321,1.);
#1333=VECTOR('',#4326,0.4);
#1334=VECTOR('',#4331,1.);
#1335=VECTOR('',#4334,1.);
#1336=VECTOR('',#4345,1.);
#1337=VECTOR('',#4348,1.);
#1338=VECTOR('',#4353,1.);
#1339=VECTOR('',#4356,1.);
#1340=VECTOR('',#4361,1.);
#1341=VECTOR('',#4364,1.);
#1342=VECTOR('',#4369,1.);
#1343=VECTOR('',#4372,1.);
#1344=VECTOR('',#4377,1.);
#1345=VECTOR('',#4380,1.);
#1346=VECTOR('',#4385,1.);
#1347=VECTOR('',#4388,1.);
#1348=VECTOR('',#4433,1.);
#1349=VECTOR('',#4434,1.);
#1350=VECTOR('',#4435,1.);
#1351=VECTOR('',#4436,1.);
#1352=VECTOR('',#4439,1.);
#1353=VECTOR('',#4440,1.);
#1354=VECTOR('',#4441,1.);
#1355=VECTOR('',#4444,1.);
#1356=VECTOR('',#4445,1.);
#1357=VECTOR('',#4446,1.);
#1358=VECTOR('',#4449,1.);
#1359=VECTOR('',#4450,1.);
#1360=VECTOR('',#4451,1.);
#1361=VECTOR('',#4454,1.);
#1362=VECTOR('',#4455,1.);
#1363=VECTOR('',#4456,1.);
#1364=VECTOR('',#4459,1.);
#1365=VECTOR('',#4460,1.);
#1366=VECTOR('',#4467,0.425);
#1367=CIRCLE('',#3309,0.275);
#1368=CIRCLE('',#3310,0.275);
#1369=CIRCLE('',#3312,0.275);
#1370=CIRCLE('',#3313,0.275);
#1371=CIRCLE('',#3315,0.425);
#1372=CIRCLE('',#3316,0.425);
#1373=CIRCLE('',#3365,0.21);
#1374=CIRCLE('',#3366,0.21);
#1375=CIRCLE('',#3381,0.2117);
#1376=CIRCLE('',#3390,0.2117);
#1377=CIRCLE('',#3391,0.2117);
#1378=CIRCLE('',#3393,0.2117);
#1379=CIRCLE('',#3400,0.285);
#1380=CIRCLE('',#3401,0.265);
#1381=CIRCLE('',#3403,0.265);
#1382=CIRCLE('',#3405,0.5);
#1383=CIRCLE('',#3407,0.5);
#1384=CIRCLE('',#3419,0.24505);
#1385=CIRCLE('',#3421,0.375);
#1386=CIRCLE('',#3423,0.425);
#1387=CIRCLE('',#3425,0.425);
#1388=CIRCLE('',#3427,0.395);
#1389=CIRCLE('',#3429,0.27);
#1390=CIRCLE('',#3431,0.24505);
#1391=CIRCLE('',#3437,0.425);
#1392=CIRCLE('',#3438,0.425);
#1393=CIRCLE('',#3440,0.425000000000001);
#1394=CIRCLE('',#3441,0.425000000000001);
#1395=CIRCLE('',#3443,1.5);
#1396=CIRCLE('',#3444,1.5);
#1397=CIRCLE('',#3447,1.5);
#1398=CIRCLE('',#3450,1.5);
#1399=CIRCLE('',#3454,0.3933);
#1400=CIRCLE('',#3455,0.3933);
#1401=CIRCLE('',#3457,0.32);
#1402=CIRCLE('',#3460,0.6175);
#1403=CIRCLE('',#3481,0.329999999999998);
#1404=CIRCLE('',#3482,0.329999999999998);
#1405=CIRCLE('',#3484,0.329999999999998);
#1406=CIRCLE('',#3485,0.329999999999998);
#1407=CIRCLE('',#3487,0.329999999999998);
#1408=CIRCLE('',#3488,0.329999999999998);
#1409=CIRCLE('',#3490,0.329999999999998);
#1410=CIRCLE('',#3491,0.329999999999998);
#1411=CIRCLE('',#3493,0.425000000000001);
#1412=CIRCLE('',#3494,0.425000000000001);
#1413=CIRCLE('',#3502,1.5);
#1414=CIRCLE('',#3505,1.5);
#1415=CIRCLE('',#3509,0.42);
#1416=CIRCLE('',#3510,0.42);
#1417=CIRCLE('',#3512,0.8);
#1418=CIRCLE('',#3513,0.8);
#1419=CIRCLE('',#3518,0.6175);
#1420=CIRCLE('',#3520,0.6175);
#1421=CIRCLE('',#3525,0.338975);
#1422=CIRCLE('',#3526,0.338975);
#1423=CIRCLE('',#3534,0.4);
#1424=CIRCLE('',#3535,0.4);
#1425=CIRCLE('',#3537,0.4);
#1426=CIRCLE('',#3538,0.4);
#1427=CIRCLE('',#3540,0.4);
#1428=CIRCLE('',#3541,0.4);
#1429=CIRCLE('',#3543,0.4);
#1430=CIRCLE('',#3544,0.4);
#1431=CIRCLE('',#3546,0.4);
#1432=CIRCLE('',#3547,0.4);
#1433=CIRCLE('',#3549,0.4);
#1434=CIRCLE('',#3550,0.4);
#1435=CIRCLE('',#3552,1.8);
#1436=CIRCLE('',#3553,1.8);
#1437=CIRCLE('',#3554,1.8);
#1438=CIRCLE('',#3555,1.8);
#1439=CIRCLE('',#3556,1.8);
#1440=CIRCLE('',#3557,1.8);
#1441=CIRCLE('',#3558,0.425);
#1442=CIRCLE('',#3560,1.8);
#1443=CIRCLE('',#3562,1.8);
#1444=CIRCLE('',#3564,1.8);
#1445=CIRCLE('',#3566,1.8);
#1446=CIRCLE('',#3568,1.8);
#1447=CIRCLE('',#3570,1.8);
#1448=CIRCLE('',#3578,0.425);
#1449=VERTEX_POINT('',#4522);
#1450=VERTEX_POINT('',#4524);
#1451=VERTEX_POINT('',#4528);
#1452=VERTEX_POINT('',#4530);
#1453=VERTEX_POINT('',#4534);
#1454=VERTEX_POINT('',#4536);
#1455=VERTEX_POINT('',#4540);
#1456=VERTEX_POINT('',#4541);
#1457=VERTEX_POINT('',#4543);
#1458=VERTEX_POINT('',#4545);
#1459=VERTEX_POINT('',#4549);
#1460=VERTEX_POINT('',#4550);
#1461=VERTEX_POINT('',#4552);
#1462=VERTEX_POINT('',#4554);
#1463=VERTEX_POINT('',#4563);
#1464=VERTEX_POINT('',#4565);
#1465=VERTEX_POINT('',#4567);
#1466=VERTEX_POINT('',#4569);
#1467=VERTEX_POINT('',#4573);
#1468=VERTEX_POINT('',#4574);
#1469=VERTEX_POINT('',#4579);
#1470=VERTEX_POINT('',#4583);
#1471=VERTEX_POINT('',#4591);
#1472=VERTEX_POINT('',#4592);
#1473=VERTEX_POINT('',#4594);
#1474=VERTEX_POINT('',#4596);
#1475=VERTEX_POINT('',#4600);
#1476=VERTEX_POINT('',#4602);
#1477=VERTEX_POINT('',#4606);
#1478=VERTEX_POINT('',#4608);
#1479=VERTEX_POINT('',#4612);
#1480=VERTEX_POINT('',#4614);
#1481=VERTEX_POINT('',#4618);
#1482=VERTEX_POINT('',#4620);
#1483=VERTEX_POINT('',#4624);
#1484=VERTEX_POINT('',#4626);
#1485=VERTEX_POINT('',#4630);
#1486=VERTEX_POINT('',#4632);
#1487=VERTEX_POINT('',#4636);
#1488=VERTEX_POINT('',#4638);
#1489=VERTEX_POINT('',#4642);
#1490=VERTEX_POINT('',#4644);
#1491=VERTEX_POINT('',#4648);
#1492=VERTEX_POINT('',#4649);
#1493=VERTEX_POINT('',#4651);
#1494=VERTEX_POINT('',#4653);
#1495=VERTEX_POINT('',#4657);
#1496=VERTEX_POINT('',#4659);
#1497=VERTEX_POINT('',#4663);
#1498=VERTEX_POINT('',#4665);
#1499=VERTEX_POINT('',#4669);
#1500=VERTEX_POINT('',#4671);
#1501=VERTEX_POINT('',#4675);
#1502=VERTEX_POINT('',#4677);
#1503=VERTEX_POINT('',#4681);
#1504=VERTEX_POINT('',#4683);
#1505=VERTEX_POINT('',#4687);
#1506=VERTEX_POINT('',#4689);
#1507=VERTEX_POINT('',#4693);
#1508=VERTEX_POINT('',#4695);
#1509=VERTEX_POINT('',#4699);
#1510=VERTEX_POINT('',#4701);
#1511=VERTEX_POINT('',#4705);
#1512=VERTEX_POINT('',#4706);
#1513=VERTEX_POINT('',#4708);
#1514=VERTEX_POINT('',#4710);
#1515=VERTEX_POINT('',#4714);
#1516=VERTEX_POINT('',#4716);
#1517=VERTEX_POINT('',#4720);
#1518=VERTEX_POINT('',#4722);
#1519=VERTEX_POINT('',#4726);
#1520=VERTEX_POINT('',#4728);
#1521=VERTEX_POINT('',#4732);
#1522=VERTEX_POINT('',#4734);
#1523=VERTEX_POINT('',#4738);
#1524=VERTEX_POINT('',#4740);
#1525=VERTEX_POINT('',#4744);
#1526=VERTEX_POINT('',#4746);
#1527=VERTEX_POINT('',#4750);
#1528=VERTEX_POINT('',#4752);
#1529=VERTEX_POINT('',#4756);
#1530=VERTEX_POINT('',#4758);
#1531=VERTEX_POINT('',#4762);
#1532=VERTEX_POINT('',#4763);
#1533=VERTEX_POINT('',#4765);
#1534=VERTEX_POINT('',#4767);
#1535=VERTEX_POINT('',#4771);
#1536=VERTEX_POINT('',#4773);
#1537=VERTEX_POINT('',#4777);
#1538=VERTEX_POINT('',#4779);
#1539=VERTEX_POINT('',#4783);
#1540=VERTEX_POINT('',#4785);
#1541=VERTEX_POINT('',#4789);
#1542=VERTEX_POINT('',#4791);
#1543=VERTEX_POINT('',#4795);
#1544=VERTEX_POINT('',#4797);
#1545=VERTEX_POINT('',#4801);
#1546=VERTEX_POINT('',#4803);
#1547=VERTEX_POINT('',#4807);
#1548=VERTEX_POINT('',#4809);
#1549=VERTEX_POINT('',#4813);
#1550=VERTEX_POINT('',#4815);
#1551=VERTEX_POINT('',#4819);
#1552=VERTEX_POINT('',#4821);
#1553=VERTEX_POINT('',#4825);
#1554=VERTEX_POINT('',#4827);
#1555=VERTEX_POINT('',#4831);
#1556=VERTEX_POINT('',#4833);
#1557=VERTEX_POINT('',#4840);
#1558=VERTEX_POINT('',#4842);
#1559=VERTEX_POINT('',#4849);
#1560=VERTEX_POINT('',#4851);
#1561=VERTEX_POINT('',#4864);
#1562=VERTEX_POINT('',#4865);
#1563=VERTEX_POINT('',#4867);
#1564=VERTEX_POINT('',#4869);
#1565=VERTEX_POINT('',#4873);
#1566=VERTEX_POINT('',#4875);
#1567=VERTEX_POINT('',#4879);
#1568=VERTEX_POINT('',#4881);
#1569=VERTEX_POINT('',#4884);
#1570=VERTEX_POINT('',#4887);
#1571=VERTEX_POINT('',#4889);
#1572=VERTEX_POINT('',#4891);
#1573=VERTEX_POINT('',#4893);
#1574=VERTEX_POINT('',#4895);
#1575=VERTEX_POINT('',#4897);
#1576=VERTEX_POINT('',#4901);
#1577=VERTEX_POINT('',#4905);
#1578=VERTEX_POINT('',#4909);
#1579=VERTEX_POINT('',#4911);
#1580=VERTEX_POINT('',#4913);
#1581=VERTEX_POINT('',#4915);
#1582=VERTEX_POINT('',#4921);
#1583=VERTEX_POINT('',#4923);
#1584=VERTEX_POINT('',#4927);
#1585=VERTEX_POINT('',#4930);
#1586=VERTEX_POINT('',#4932);
#1587=VERTEX_POINT('',#4944);
#1588=VERTEX_POINT('',#4946);
#1589=VERTEX_POINT('',#4950);
#1590=VERTEX_POINT('',#4954);
#1591=VERTEX_POINT('',#4957);
#1592=VERTEX_POINT('',#4963);
#1593=VERTEX_POINT('',#4964);
#1594=VERTEX_POINT('',#4966);
#1595=VERTEX_POINT('',#4968);
#1596=VERTEX_POINT('',#4972);
#1597=VERTEX_POINT('',#4974);
#1598=VERTEX_POINT('',#4978);
#1599=VERTEX_POINT('',#4980);
#1600=VERTEX_POINT('',#4984);
#1601=VERTEX_POINT('',#4986);
#1602=VERTEX_POINT('',#4990);
#1603=VERTEX_POINT('',#4992);
#1604=VERTEX_POINT('',#5001);
#1605=VERTEX_POINT('',#5004);
#1606=VERTEX_POINT('',#5007);
#1607=VERTEX_POINT('',#5011);
#1608=VERTEX_POINT('',#5015);
#1609=VERTEX_POINT('',#5019);
#1610=VERTEX_POINT('',#5022);
#1611=VERTEX_POINT('',#5031);
#1612=VERTEX_POINT('',#5033);
#1613=VERTEX_POINT('',#5037);
#1614=VERTEX_POINT('',#5039);
#1615=VERTEX_POINT('',#5043);
#1616=VERTEX_POINT('',#5044);
#1617=VERTEX_POINT('',#5046);
#1618=VERTEX_POINT('',#5048);
#1619=VERTEX_POINT('',#5052);
#1620=VERTEX_POINT('',#5054);
#1621=VERTEX_POINT('',#5058);
#1622=VERTEX_POINT('',#5062);
#1623=VERTEX_POINT('',#5070);
#1624=VERTEX_POINT('',#5072);
#1625=VERTEX_POINT('',#5076);
#1626=VERTEX_POINT('',#5081);
#1627=VERTEX_POINT('',#5083);
#1628=VERTEX_POINT('',#5085);
#1629=VERTEX_POINT('',#5089);
#1630=VERTEX_POINT('',#5093);
#1631=VERTEX_POINT('',#5097);
#1632=VERTEX_POINT('',#5101);
#1633=VERTEX_POINT('',#5109);
#1634=VERTEX_POINT('',#5111);
#1635=VERTEX_POINT('',#5115);
#1636=VERTEX_POINT('',#5119);
#1637=VERTEX_POINT('',#5123);
#1638=VERTEX_POINT('',#5127);
#1639=VERTEX_POINT('',#5146);
#1640=VERTEX_POINT('',#5148);
#1641=VERTEX_POINT('',#5152);
#1642=VERTEX_POINT('',#5154);
#1643=VERTEX_POINT('',#5158);
#1644=VERTEX_POINT('',#5160);
#1645=VERTEX_POINT('',#5164);
#1646=VERTEX_POINT('',#5166);
#1647=VERTEX_POINT('',#5170);
#1648=VERTEX_POINT('',#5172);
#1649=VERTEX_POINT('',#5176);
#1650=VERTEX_POINT('',#5177);
#1651=VERTEX_POINT('',#5179);
#1652=VERTEX_POINT('',#5181);
#1653=VERTEX_POINT('',#5185);
#1654=VERTEX_POINT('',#5186);
#1655=VERTEX_POINT('',#5188);
#1656=VERTEX_POINT('',#5190);
#1657=VERTEX_POINT('',#5194);
#1658=VERTEX_POINT('',#5195);
#1659=VERTEX_POINT('',#5200);
#1660=VERTEX_POINT('',#5202);
#1661=VERTEX_POINT('',#5209);
#1662=VERTEX_POINT('',#5211);
#1663=VERTEX_POINT('',#5215);
#1664=VERTEX_POINT('',#5219);
#1665=VERTEX_POINT('',#5227);
#1666=VERTEX_POINT('',#5229);
#1667=VERTEX_POINT('',#5233);
#1668=VERTEX_POINT('',#5235);
#1669=VERTEX_POINT('',#5242);
#1670=VERTEX_POINT('',#5243);
#1671=VERTEX_POINT('',#5247);
#1672=VERTEX_POINT('',#5251);
#1673=VERTEX_POINT('',#5254);
#1674=VERTEX_POINT('',#5258);
#1675=VERTEX_POINT('',#5262);
#1676=VERTEX_POINT('',#5270);
#1677=VERTEX_POINT('',#5272);
#1678=VERTEX_POINT('',#5274);
#1679=VERTEX_POINT('',#5278);
#1680=VERTEX_POINT('',#5282);
#1681=VERTEX_POINT('',#5286);
#1682=VERTEX_POINT('',#5290);
#1683=VERTEX_POINT('',#5305);
#1684=VERTEX_POINT('',#5307);
#1685=VERTEX_POINT('',#5319);
#1686=VERTEX_POINT('',#5320);
#1687=VERTEX_POINT('',#5322);
#1688=VERTEX_POINT('',#5324);
#1689=VERTEX_POINT('',#5328);
#1690=VERTEX_POINT('',#5329);
#1691=VERTEX_POINT('',#5331);
#1692=VERTEX_POINT('',#5333);
#1693=VERTEX_POINT('',#5337);
#1694=VERTEX_POINT('',#5338);
#1695=VERTEX_POINT('',#5340);
#1696=VERTEX_POINT('',#5342);
#1697=VERTEX_POINT('',#5346);
#1698=VERTEX_POINT('',#5347);
#1699=VERTEX_POINT('',#5349);
#1700=VERTEX_POINT('',#5351);
#1701=VERTEX_POINT('',#5355);
#1702=VERTEX_POINT('',#5356);
#1703=VERTEX_POINT('',#5358);
#1704=VERTEX_POINT('',#5360);
#1705=VERTEX_POINT('',#5364);
#1706=VERTEX_POINT('',#5365);
#1707=VERTEX_POINT('',#5367);
#1708=VERTEX_POINT('',#5369);
#1709=VERTEX_POINT('',#5379);
#1710=VERTEX_POINT('',#5394);
#1711=VERTEX_POINT('',#5395);
#1712=VERTEX_POINT('',#5397);
#1713=VERTEX_POINT('',#5399);
#1714=VERTEX_POINT('',#5403);
#1715=VERTEX_POINT('',#5405);
#1716=VERTEX_POINT('',#5409);
#1717=VERTEX_POINT('',#5411);
#1718=VERTEX_POINT('',#5415);
#1719=VERTEX_POINT('',#5417);
#1720=VERTEX_POINT('',#5421);
#1721=VERTEX_POINT('',#5423);
#1722=VERTEX_POINT('',#5430);
#1723=EDGE_CURVE('',#1449,#1449,#1367,.T.);
#1724=EDGE_CURVE('',#1449,#1450,#741,.T.);
#1725=EDGE_CURVE('',#1450,#1450,#1368,.T.);
#1726=EDGE_CURVE('',#1451,#1451,#1369,.T.);
#1727=EDGE_CURVE('',#1451,#1452,#742,.T.);
#1728=EDGE_CURVE('',#1452,#1452,#1370,.T.);
#1729=EDGE_CURVE('',#1453,#1453,#1371,.T.);
#1730=EDGE_CURVE('',#1453,#1454,#743,.T.);
#1731=EDGE_CURVE('',#1454,#1454,#1372,.T.);
#1732=EDGE_CURVE('',#1455,#1456,#744,.T.);
#1733=EDGE_CURVE('',#1455,#1457,#745,.T.);
#1734=EDGE_CURVE('',#1458,#1457,#746,.T.);
#1735=EDGE_CURVE('',#1456,#1458,#747,.T.);
#1736=EDGE_CURVE('',#1459,#1460,#748,.T.);
#1737=EDGE_CURVE('',#1461,#1459,#749,.T.);
#1738=EDGE_CURVE('',#1462,#1461,#750,.T.);
#1739=EDGE_CURVE('',#1460,#1462,#751,.T.);
#1740=EDGE_CURVE('',#1460,#1455,#752,.T.);
#1741=EDGE_CURVE('',#1457,#1462,#753,.T.);
#1742=EDGE_CURVE('',#1459,#1456,#754,.T.);
#1743=EDGE_CURVE('',#1458,#1463,#755,.T.);
#1744=EDGE_CURVE('',#1463,#1464,#756,.T.);
#1745=EDGE_CURVE('',#1464,#1465,#757,.T.);
#1746=EDGE_CURVE('',#1465,#1466,#758,.T.);
#1747=EDGE_CURVE('',#1466,#1461,#759,.T.);
#1748=EDGE_CURVE('',#1467,#1468,#760,.T.);
#1749=EDGE_CURVE('',#1468,#1463,#761,.T.);
#1750=EDGE_CURVE('',#1467,#1466,#762,.T.);
#1751=EDGE_CURVE('',#1469,#1467,#763,.T.);
#1752=EDGE_CURVE('',#1469,#1465,#764,.T.);
#1753=EDGE_CURVE('',#1470,#1469,#765,.T.);
#1754=EDGE_CURVE('',#1470,#1464,#766,.T.);
#1755=EDGE_CURVE('',#1468,#1470,#767,.T.);
#1756=EDGE_CURVE('',#1471,#1472,#768,.T.);
#1757=EDGE_CURVE('',#1471,#1473,#769,.T.);
#1758=EDGE_CURVE('',#1474,#1473,#770,.T.);
#1759=EDGE_CURVE('',#1472,#1474,#771,.T.);
#1760=EDGE_CURVE('',#1475,#1471,#772,.T.);
#1761=EDGE_CURVE('',#1475,#1476,#773,.T.);
#1762=EDGE_CURVE('',#1473,#1476,#774,.T.);
#1763=EDGE_CURVE('',#1477,#1475,#775,.T.);
#1764=EDGE_CURVE('',#1477,#1478,#776,.T.);
#1765=EDGE_CURVE('',#1476,#1478,#777,.T.);
#1766=EDGE_CURVE('',#1479,#1477,#778,.T.);
#1767=EDGE_CURVE('',#1479,#1480,#779,.T.);
#1768=EDGE_CURVE('',#1478,#1480,#780,.T.);
#1769=EDGE_CURVE('',#1481,#1479,#781,.T.);
#1770=EDGE_CURVE('',#1481,#1482,#782,.T.);
#1771=EDGE_CURVE('',#1480,#1482,#783,.T.);
#1772=EDGE_CURVE('',#1483,#1481,#784,.T.);
#1773=EDGE_CURVE('',#1483,#1484,#785,.T.);
#1774=EDGE_CURVE('',#1482,#1484,#786,.T.);
#1775=EDGE_CURVE('',#1485,#1483,#787,.T.);
#1776=EDGE_CURVE('',#1485,#1486,#788,.T.);
#1777=EDGE_CURVE('',#1484,#1486,#789,.T.);
#1778=EDGE_CURVE('',#1487,#1485,#790,.T.);
#1779=EDGE_CURVE('',#1487,#1488,#791,.T.);
#1780=EDGE_CURVE('',#1486,#1488,#792,.T.);
#1781=EDGE_CURVE('',#1489,#1487,#793,.T.);
#1782=EDGE_CURVE('',#1490,#1489,#794,.T.);
#1783=EDGE_CURVE('',#1488,#1490,#795,.T.);
#1784=EDGE_CURVE('',#1491,#1492,#796,.T.);
#1785=EDGE_CURVE('',#1491,#1493,#797,.T.);
#1786=EDGE_CURVE('',#1494,#1493,#798,.T.);
#1787=EDGE_CURVE('',#1492,#1494,#799,.T.);
#1788=EDGE_CURVE('',#1495,#1491,#800,.T.);
#1789=EDGE_CURVE('',#1495,#1496,#801,.T.);
#1790=EDGE_CURVE('',#1493,#1496,#802,.T.);
#1791=EDGE_CURVE('',#1497,#1495,#803,.T.);
#1792=EDGE_CURVE('',#1497,#1498,#804,.T.);
#1793=EDGE_CURVE('',#1496,#1498,#805,.T.);
#1794=EDGE_CURVE('',#1499,#1497,#806,.T.);
#1795=EDGE_CURVE('',#1499,#1500,#807,.T.);
#1796=EDGE_CURVE('',#1498,#1500,#808,.T.);
#1797=EDGE_CURVE('',#1501,#1499,#809,.T.);
#1798=EDGE_CURVE('',#1501,#1502,#810,.T.);
#1799=EDGE_CURVE('',#1500,#1502,#811,.T.);
#1800=EDGE_CURVE('',#1503,#1501,#812,.T.);
#1801=EDGE_CURVE('',#1503,#1504,#813,.T.);
#1802=EDGE_CURVE('',#1502,#1504,#814,.T.);
#1803=EDGE_CURVE('',#1505,#1503,#815,.T.);
#1804=EDGE_CURVE('',#1505,#1506,#816,.T.);
#1805=EDGE_CURVE('',#1504,#1506,#817,.T.);
#1806=EDGE_CURVE('',#1507,#1505,#818,.T.);
#1807=EDGE_CURVE('',#1507,#1508,#819,.T.);
#1808=EDGE_CURVE('',#1506,#1508,#820,.T.);
#1809=EDGE_CURVE('',#1509,#1507,#821,.T.);
#1810=EDGE_CURVE('',#1510,#1509,#822,.T.);
#1811=EDGE_CURVE('',#1508,#1510,#823,.T.);
#1812=EDGE_CURVE('',#1511,#1512,#824,.T.);
#1813=EDGE_CURVE('',#1511,#1513,#825,.T.);
#1814=EDGE_CURVE('',#1514,#1513,#826,.T.);
#1815=EDGE_CURVE('',#1512,#1514,#827,.T.);
#1816=EDGE_CURVE('',#1515,#1511,#828,.T.);
#1817=EDGE_CURVE('',#1515,#1516,#829,.T.);
#1818=EDGE_CURVE('',#1513,#1516,#830,.T.);
#1819=EDGE_CURVE('',#1517,#1515,#831,.T.);
#1820=EDGE_CURVE('',#1517,#1518,#832,.T.);
#1821=EDGE_CURVE('',#1516,#1518,#833,.T.);
#1822=EDGE_CURVE('',#1519,#1517,#834,.T.);
#1823=EDGE_CURVE('',#1519,#1520,#835,.T.);
#1824=EDGE_CURVE('',#1518,#1520,#836,.T.);
#1825=EDGE_CURVE('',#1521,#1519,#837,.T.);
#1826=EDGE_CURVE('',#1521,#1522,#838,.T.);
#1827=EDGE_CURVE('',#1520,#1522,#839,.T.);
#1828=EDGE_CURVE('',#1523,#1521,#840,.T.);
#1829=EDGE_CURVE('',#1523,#1524,#841,.T.);
#1830=EDGE_CURVE('',#1522,#1524,#842,.T.);
#1831=EDGE_CURVE('',#1525,#1523,#843,.T.);
#1832=EDGE_CURVE('',#1525,#1526,#844,.T.);
#1833=EDGE_CURVE('',#1524,#1526,#845,.T.);
#1834=EDGE_CURVE('',#1527,#1525,#846,.T.);
#1835=EDGE_CURVE('',#1527,#1528,#847,.T.);
#1836=EDGE_CURVE('',#1526,#1528,#848,.T.);
#1837=EDGE_CURVE('',#1529,#1527,#849,.T.);
#1838=EDGE_CURVE('',#1530,#1529,#850,.T.);
#1839=EDGE_CURVE('',#1528,#1530,#851,.T.);
#1840=EDGE_CURVE('',#1531,#1532,#852,.T.);
#1841=EDGE_CURVE('',#1531,#1533,#853,.T.);
#1842=EDGE_CURVE('',#1534,#1533,#854,.T.);
#1843=EDGE_CURVE('',#1532,#1534,#855,.T.);
#1844=EDGE_CURVE('',#1535,#1531,#856,.T.);
#1845=EDGE_CURVE('',#1535,#1536,#857,.T.);
#1846=EDGE_CURVE('',#1533,#1536,#858,.T.);
#1847=EDGE_CURVE('',#1537,#1535,#859,.T.);
#1848=EDGE_CURVE('',#1537,#1538,#860,.T.);
#1849=EDGE_CURVE('',#1536,#1538,#861,.T.);
#1850=EDGE_CURVE('',#1539,#1537,#862,.T.);
#1851=EDGE_CURVE('',#1539,#1540,#863,.T.);
#1852=EDGE_CURVE('',#1538,#1540,#864,.T.);
#1853=EDGE_CURVE('',#1541,#1539,#865,.T.);
#1854=EDGE_CURVE('',#1541,#1542,#866,.T.);
#1855=EDGE_CURVE('',#1540,#1542,#867,.T.);
#1856=EDGE_CURVE('',#1543,#1541,#868,.T.);
#1857=EDGE_CURVE('',#1543,#1544,#869,.T.);
#1858=EDGE_CURVE('',#1542,#1544,#870,.T.);
#1859=EDGE_CURVE('',#1545,#1543,#871,.T.);
#1860=EDGE_CURVE('',#1545,#1546,#872,.T.);
#1861=EDGE_CURVE('',#1544,#1546,#873,.T.);
#1862=EDGE_CURVE('',#1547,#1545,#874,.T.);
#1863=EDGE_CURVE('',#1547,#1548,#875,.T.);
#1864=EDGE_CURVE('',#1546,#1548,#876,.T.);
#1865=EDGE_CURVE('',#1549,#1547,#877,.T.);
#1866=EDGE_CURVE('',#1550,#1549,#878,.T.);
#1867=EDGE_CURVE('',#1548,#1550,#879,.T.);
#1868=EDGE_CURVE('',#1551,#1551,#1373,.T.);
#1869=EDGE_CURVE('',#1551,#1552,#880,.T.);
#1870=EDGE_CURVE('',#1552,#1552,#1374,.T.);
#1871=EDGE_CURVE('',#1489,#1553,#881,.T.);
#1872=EDGE_CURVE('',#1553,#1554,#882,.T.);
#1873=EDGE_CURVE('',#1490,#1554,#883,.T.);
#1874=EDGE_CURVE('',#1555,#1474,#884,.T.);
#1875=EDGE_CURVE('',#1556,#1555,#885,.T.);
#1876=EDGE_CURVE('',#1556,#1472,#886,.T.);
#1877=EDGE_CURVE('',#1509,#1556,#887,.T.);
#1878=EDGE_CURVE('',#1510,#1555,#888,.T.);
#1879=EDGE_CURVE('',#1557,#1494,#889,.T.);
#1880=EDGE_CURVE('',#1558,#1557,#890,.T.);
#1881=EDGE_CURVE('',#1558,#1492,#891,.T.);
#1882=EDGE_CURVE('',#1529,#1558,#892,.T.);
#1883=EDGE_CURVE('',#1530,#1557,#893,.T.);
#1884=EDGE_CURVE('',#1559,#1514,#894,.T.);
#1885=EDGE_CURVE('',#1560,#1559,#895,.T.);
#1886=EDGE_CURVE('',#1560,#1512,#896,.T.);
#1887=EDGE_CURVE('',#1549,#1560,#897,.T.);
#1888=EDGE_CURVE('',#1550,#1559,#898,.T.);
#1889=EDGE_CURVE('',#1554,#1534,#899,.T.);
#1890=EDGE_CURVE('',#1553,#1532,#900,.T.);
#1891=EDGE_CURVE('',#1561,#1562,#901,.T.);
#1892=EDGE_CURVE('',#1563,#1561,#902,.T.);
#1893=EDGE_CURVE('',#1564,#1563,#903,.T.);
#1894=EDGE_CURVE('',#1562,#1564,#904,.T.);
#1895=EDGE_CURVE('',#1563,#1565,#905,.T.);
#1896=EDGE_CURVE('',#1566,#1565,#906,.T.);
#1897=EDGE_CURVE('',#1564,#1566,#907,.T.);
#1898=EDGE_CURVE('',#1565,#1567,#908,.T.);
#1899=EDGE_CURVE('',#1567,#1568,#909,.T.);
#1900=EDGE_CURVE('',#1568,#1566,#910,.T.);
#1901=EDGE_CURVE('',#1569,#1569,#1375,.T.);
#1902=EDGE_CURVE('',#1570,#1561,#911,.T.);
#1903=EDGE_CURVE('',#1571,#1570,#912,.T.);
#1904=EDGE_CURVE('',#1571,#1572,#913,.T.);
#1905=EDGE_CURVE('',#1573,#1572,#914,.T.);
#1906=EDGE_CURVE('',#1573,#1574,#915,.T.);
#1907=EDGE_CURVE('',#1574,#1575,#916,.T.);
#1908=EDGE_CURVE('',#1575,#1567,#917,.T.);
#1909=EDGE_CURVE('',#1575,#1576,#918,.T.);
#1910=EDGE_CURVE('',#1576,#1568,#919,.T.);
#1911=EDGE_CURVE('',#1577,#1574,#920,.T.);
#1912=EDGE_CURVE('',#1576,#1577,#921,.T.);
#1913=EDGE_CURVE('',#1578,#1577,#922,.T.);
#1914=EDGE_CURVE('',#1579,#1578,#923,.T.);
#1915=EDGE_CURVE('',#1579,#1580,#924,.T.);
#1916=EDGE_CURVE('',#1581,#1580,#925,.T.);
#1917=EDGE_CURVE('',#1581,#1562,#926,.T.);
#1918=EDGE_CURVE('',#1578,#1573,#927,.T.);
#1919=EDGE_CURVE('',#1572,#1582,#928,.T.);
#1920=EDGE_CURVE('',#1582,#1583,#171,.T.);
#1921=EDGE_CURVE('',#1583,#1579,#929,.T.);
#1922=EDGE_CURVE('',#1584,#1582,#1376,.F.);
#1923=EDGE_CURVE('',#1584,#1569,#930,.T.);
#1924=EDGE_CURVE('',#1585,#1584,#1377,.F.);
#1925=EDGE_CURVE('',#1586,#1585,#172,.T.);
#1926=EDGE_CURVE('',#1583,#1586,#1378,.F.);
#1927=EDGE_CURVE('',#1585,#1571,#931,.T.);
#1928=EDGE_CURVE('',#1580,#1586,#932,.T.);
#1929=EDGE_CURVE('',#1570,#1581,#933,.T.);
#1930=EDGE_CURVE('',#1587,#1587,#1379,.T.);
#1931=EDGE_CURVE('',#1587,#1588,#934,.T.);
#1932=EDGE_CURVE('',#1588,#1588,#1380,.T.);
#1933=EDGE_CURVE('',#1588,#1589,#935,.T.);
#1934=EDGE_CURVE('',#1589,#1589,#1381,.T.);
#1935=EDGE_CURVE('',#1590,#1590,#1382,.T.);
#1936=EDGE_CURVE('',#1590,#1591,#936,.T.);
#1937=EDGE_CURVE('',#1591,#1591,#1383,.T.);
#1938=EDGE_CURVE('',#1592,#1593,#937,.T.);
#1939=EDGE_CURVE('',#1593,#1594,#938,.T.);
#1940=EDGE_CURVE('',#1594,#1595,#939,.T.);
#1941=EDGE_CURVE('',#1592,#1595,#940,.T.);
#1942=EDGE_CURVE('',#1593,#1596,#941,.T.);
#1943=EDGE_CURVE('',#1596,#1597,#942,.T.);
#1944=EDGE_CURVE('',#1597,#1594,#943,.T.);
#1945=EDGE_CURVE('',#1596,#1598,#944,.T.);
#1946=EDGE_CURVE('',#1598,#1599,#945,.T.);
#1947=EDGE_CURVE('',#1599,#1597,#946,.T.);
#1948=EDGE_CURVE('',#1598,#1600,#947,.T.);
#1949=EDGE_CURVE('',#1600,#1601,#948,.T.);
#1950=EDGE_CURVE('',#1601,#1599,#949,.T.);
#1951=EDGE_CURVE('',#1600,#1602,#950,.T.);
#1952=EDGE_CURVE('',#1602,#1603,#951,.T.);
#1953=EDGE_CURVE('',#1603,#1601,#952,.T.);
#1954=EDGE_CURVE('',#1602,#1592,#953,.T.);
#1955=EDGE_CURVE('',#1595,#1603,#954,.T.);
#1956=EDGE_CURVE('',#1604,#1604,#1384,.T.);
#1957=EDGE_CURVE('',#1605,#1605,#1385,.T.);
#1958=EDGE_CURVE('',#1606,#1606,#1386,.T.);
#1959=EDGE_CURVE('',#1606,#1605,#955,.T.);
#1960=EDGE_CURVE('',#1607,#1607,#1387,.T.);
#1961=EDGE_CURVE('',#1607,#1606,#956,.T.);
#1962=EDGE_CURVE('',#1608,#1608,#1388,.T.);
#1963=EDGE_CURVE('',#1608,#1607,#957,.T.);
#1964=EDGE_CURVE('',#1609,#1609,#1389,.T.);
#1965=EDGE_CURVE('',#1610,#1610,#1390,.F.);
#1966=EDGE_CURVE('',#1610,#1609,#958,.T.);
#1967=EDGE_CURVE('',#1604,#1610,#959,.T.);
#1968=EDGE_CURVE('',#1611,#1611,#1391,.T.);
#1969=EDGE_CURVE('',#1611,#1612,#960,.T.);
#1970=EDGE_CURVE('',#1612,#1612,#1392,.T.);
#1971=EDGE_CURVE('',#1613,#1613,#1393,.T.);
#1972=EDGE_CURVE('',#1613,#1614,#961,.T.);
#1973=EDGE_CURVE('',#1614,#1614,#1394,.T.);
#1974=EDGE_CURVE('',#1615,#1616,#962,.T.);
#1975=EDGE_CURVE('',#1617,#1615,#1395,.T.);
#1976=EDGE_CURVE('',#1618,#1617,#963,.T.);
#1977=EDGE_CURVE('',#1618,#1616,#1396,.T.);
#1978=EDGE_CURVE('',#1619,#1616,#964,.T.);
#1979=EDGE_CURVE('',#1620,#1619,#965,.T.);
#1980=EDGE_CURVE('',#1615,#1620,#966,.T.);
#1981=EDGE_CURVE('',#1618,#1621,#967,.T.);
#1982=EDGE_CURVE('',#1619,#1621,#1397,.T.);
#1983=EDGE_CURVE('',#1622,#1617,#968,.T.);
#1984=EDGE_CURVE('',#1621,#1622,#969,.T.);
#1985=EDGE_CURVE('',#1620,#1622,#1398,.T.);
#1986=EDGE_CURVE('',#1623,#1623,#1399,.F.);
#1987=EDGE_CURVE('',#1623,#1624,#970,.T.);
#1988=EDGE_CURVE('',#1624,#1624,#1400,.F.);
#1989=EDGE_CURVE('',#1625,#1625,#1401,.T.);
#1990=EDGE_CURVE('',#1625,#1623,#971,.T.);
#1991=EDGE_CURVE('',#1626,#1626,#1402,.T.);
#1992=EDGE_CURVE('',#1626,#1627,#972,.T.);
#1993=EDGE_CURVE('',#1628,#1627,#143,.T.);
#1994=EDGE_CURVE('',#1629,#1628,#144,.T.);
#1995=EDGE_CURVE('',#1630,#1629,#145,.T.);
#1996=EDGE_CURVE('',#1631,#1630,#146,.T.);
#1997=EDGE_CURVE('',#1632,#1631,#147,.T.);
#1998=EDGE_CURVE('',#1627,#1632,#148,.T.);
#1999=EDGE_CURVE('',#1633,#1631,#973,.T.);
#2000=EDGE_CURVE('',#1633,#1634,#974,.T.);
#2001=EDGE_CURVE('',#1634,#1632,#975,.T.);
#2002=EDGE_CURVE('',#1635,#1630,#976,.T.);
#2003=EDGE_CURVE('',#1635,#1633,#977,.T.);
#2004=EDGE_CURVE('',#1636,#1629,#978,.T.);
#2005=EDGE_CURVE('',#1636,#1635,#979,.T.);
#2006=EDGE_CURVE('',#1637,#1628,#980,.T.);
#2007=EDGE_CURVE('',#1637,#1636,#981,.T.);
#2008=EDGE_CURVE('',#1638,#1627,#982,.T.);
#2009=EDGE_CURVE('',#1638,#1637,#983,.T.);
#2010=EDGE_CURVE('',#1634,#1638,#984,.T.);
#2011=EDGE_CURVE('',#1639,#1639,#1403,.T.);
#2012=EDGE_CURVE('',#1639,#1640,#985,.T.);
#2013=EDGE_CURVE('',#1640,#1640,#1404,.T.);
#2014=EDGE_CURVE('',#1641,#1641,#1405,.T.);
#2015=EDGE_CURVE('',#1641,#1642,#986,.T.);
#2016=EDGE_CURVE('',#1642,#1642,#1406,.T.);
#2017=EDGE_CURVE('',#1643,#1643,#1407,.T.);
#2018=EDGE_CURVE('',#1643,#1644,#987,.T.);
#2019=EDGE_CURVE('',#1644,#1644,#1408,.T.);
#2020=EDGE_CURVE('',#1645,#1645,#1409,.T.);
#2021=EDGE_CURVE('',#1645,#1646,#988,.T.);
#2022=EDGE_CURVE('',#1646,#1646,#1410,.T.);
#2023=EDGE_CURVE('',#1647,#1647,#1411,.T.);
#2024=EDGE_CURVE('',#1647,#1648,#989,.T.);
#2025=EDGE_CURVE('',#1648,#1648,#1412,.T.);
#2026=EDGE_CURVE('',#1649,#1650,#990,.T.);
#2027=EDGE_CURVE('',#1651,#1649,#991,.T.);
#2028=EDGE_CURVE('',#1652,#1651,#992,.T.);
#2029=EDGE_CURVE('',#1650,#1652,#993,.T.);
#2030=EDGE_CURVE('',#1653,#1654,#994,.T.);
#2031=EDGE_CURVE('',#1653,#1655,#995,.T.);
#2032=EDGE_CURVE('',#1656,#1655,#996,.T.);
#2033=EDGE_CURVE('',#1654,#1656,#997,.T.);
#2034=EDGE_CURVE('',#1657,#1658,#998,.T.);
#2035=EDGE_CURVE('',#1654,#1657,#999,.T.);
#2036=EDGE_CURVE('',#1658,#1656,#1000,.T.);
#2037=EDGE_CURVE('',#1652,#1659,#1001,.T.);
#2038=EDGE_CURVE('',#1660,#1651,#1002,.T.);
#2039=EDGE_CURVE('',#1659,#1660,#1003,.T.);
#2040=EDGE_CURVE('',#1659,#1653,#1004,.T.);
#2041=EDGE_CURVE('',#1655,#1660,#1005,.T.);
#2042=EDGE_CURVE('',#1661,#1658,#1006,.T.);
#2043=EDGE_CURVE('',#1662,#1661,#1007,.T.);
#2044=EDGE_CURVE('',#1657,#1662,#1008,.T.);
#2045=EDGE_CURVE('',#1649,#1663,#1009,.T.);
#2046=EDGE_CURVE('',#1663,#1661,#1413,.T.);
#2047=EDGE_CURVE('',#1664,#1650,#1010,.T.);
#2048=EDGE_CURVE('',#1663,#1664,#1011,.T.);
#2049=EDGE_CURVE('',#1664,#1662,#1414,.T.);
#2050=EDGE_CURVE('',#1665,#1665,#1415,.T.);
#2051=EDGE_CURVE('',#1665,#1666,#1012,.T.);
#2052=EDGE_CURVE('',#1666,#1666,#1416,.T.);
#2053=EDGE_CURVE('',#1667,#1667,#1417,.T.);
#2054=EDGE_CURVE('',#1667,#1668,#1013,.T.);
#2055=EDGE_CURVE('',#1668,#1668,#1418,.T.);
#2056=EDGE_CURVE('',#1669,#1670,#149,.T.);
#2057=EDGE_CURVE('',#1671,#1669,#150,.T.);
#2058=EDGE_CURVE('',#1671,#1672,#1014,.T.);
#2059=EDGE_CURVE('',#1672,#1672,#1419,.T.);
#2060=EDGE_CURVE('',#1673,#1671,#151,.T.);
#2061=EDGE_CURVE('',#1674,#1673,#152,.T.);
#2062=EDGE_CURVE('',#1675,#1674,#153,.T.);
#2063=EDGE_CURVE('',#1670,#1675,#154,.T.);
#2064=EDGE_CURVE('',#1676,#1676,#1420,.T.);
#2065=EDGE_CURVE('',#1676,#1677,#1015,.T.);
#2066=EDGE_CURVE('',#1678,#1677,#155,.T.);
#2067=EDGE_CURVE('',#1679,#1678,#156,.T.);
#2068=EDGE_CURVE('',#1680,#1679,#157,.T.);
#2069=EDGE_CURVE('',#1681,#1680,#158,.T.);
#2070=EDGE_CURVE('',#1682,#1681,#159,.T.);
#2071=EDGE_CURVE('',#1677,#1682,#160,.T.);
#2072=EDGE_CURVE('',#1673,#1682,#1016,.T.);
#2073=EDGE_CURVE('',#1674,#1681,#1017,.T.);
#2074=EDGE_CURVE('',#1671,#1677,#1018,.T.);
#2075=EDGE_CURVE('',#1669,#1678,#1019,.T.);
#2076=EDGE_CURVE('',#1683,#1683,#1421,.F.);
#2077=EDGE_CURVE('',#1683,#1684,#1020,.T.);
#2078=EDGE_CURVE('',#1684,#1684,#1422,.F.);
#2079=EDGE_CURVE('',#1670,#1679,#1021,.T.);
#2080=EDGE_CURVE('',#1675,#1680,#1022,.T.);
#2081=EDGE_CURVE('',#1685,#1686,#1023,.T.);
#2082=EDGE_CURVE('',#1687,#1685,#1423,.T.);
#2083=EDGE_CURVE('',#1688,#1687,#1024,.T.);
#2084=EDGE_CURVE('',#1686,#1688,#1424,.T.);
#2085=EDGE_CURVE('',#1689,#1690,#1025,.T.);
#2086=EDGE_CURVE('',#1691,#1689,#1425,.T.);
#2087=EDGE_CURVE('',#1692,#1691,#1026,.T.);
#2088=EDGE_CURVE('',#1690,#1692,#1426,.T.);
#2089=EDGE_CURVE('',#1693,#1694,#1027,.T.);
#2090=EDGE_CURVE('',#1695,#1693,#1427,.T.);
#2091=EDGE_CURVE('',#1696,#1695,#1028,.T.);
#2092=EDGE_CURVE('',#1694,#1696,#1428,.T.);
#2093=EDGE_CURVE('',#1697,#1698,#1029,.T.);
#2094=EDGE_CURVE('',#1699,#1697,#1429,.T.);
#2095=EDGE_CURVE('',#1700,#1699,#1030,.T.);
#2096=EDGE_CURVE('',#1698,#1700,#1430,.T.);
#2097=EDGE_CURVE('',#1701,#1702,#1031,.T.);
#2098=EDGE_CURVE('',#1703,#1701,#1431,.T.);
#2099=EDGE_CURVE('',#1704,#1703,#1032,.T.);
#2100=EDGE_CURVE('',#1702,#1704,#1432,.T.);
#2101=EDGE_CURVE('',#1705,#1706,#1033,.T.);
#2102=EDGE_CURVE('',#1707,#1705,#1433,.T.);
#2103=EDGE_CURVE('',#1708,#1707,#1034,.T.);
#2104=EDGE_CURVE('',#1706,#1708,#1434,.T.);
#2105=EDGE_CURVE('',#1685,#1707,#1435,.T.);
#2106=EDGE_CURVE('',#1705,#1690,#1436,.T.);
#2107=EDGE_CURVE('',#1692,#1695,#1437,.T.);
#2108=EDGE_CURVE('',#1693,#1699,#1438,.T.);
#2109=EDGE_CURVE('',#1697,#1703,#1439,.T.);
#2110=EDGE_CURVE('',#1701,#1687,#1440,.T.);
#2111=EDGE_CURVE('',#1709,#1709,#1441,.T.);
#2112=EDGE_CURVE('',#1698,#1704,#1442,.T.);
#2113=EDGE_CURVE('',#1694,#1700,#1443,.T.);
#2114=EDGE_CURVE('',#1706,#1689,#1444,.T.);
#2115=EDGE_CURVE('',#1691,#1696,#1445,.T.);
#2116=EDGE_CURVE('',#1686,#1708,#1446,.T.);
#2117=EDGE_CURVE('',#1702,#1688,#1447,.T.);
#2118=EDGE_CURVE('',#1710,#1711,#1035,.T.);
#2119=EDGE_CURVE('',#1710,#1712,#1036,.T.);
#2120=EDGE_CURVE('',#1712,#1713,#1037,.T.);
#2121=EDGE_CURVE('',#1711,#1713,#1038,.T.);
#2122=EDGE_CURVE('',#1711,#1714,#1039,.T.);
#2123=EDGE_CURVE('',#1713,#1715,#1040,.T.);
#2124=EDGE_CURVE('',#1714,#1715,#1041,.T.);
#2125=EDGE_CURVE('',#1714,#1716,#1042,.T.);
#2126=EDGE_CURVE('',#1715,#1717,#1043,.T.);
#2127=EDGE_CURVE('',#1716,#1717,#1044,.T.);
#2128=EDGE_CURVE('',#1716,#1718,#1045,.T.);
#2129=EDGE_CURVE('',#1717,#1719,#1046,.T.);
#2130=EDGE_CURVE('',#1718,#1719,#1047,.T.);
#2131=EDGE_CURVE('',#1720,#1710,#1048,.T.);
#2132=EDGE_CURVE('',#1720,#1721,#1049,.T.);
#2133=EDGE_CURVE('',#1721,#1712,#1050,.T.);
#2134=EDGE_CURVE('',#1718,#1720,#1051,.T.);
#2135=EDGE_CURVE('',#1719,#1721,#1052,.T.);
#2136=EDGE_CURVE('',#1722,#1722,#1448,.T.);
#2137=EDGE_CURVE('',#1709,#1722,#1053,.T.);
#2138=ORIENTED_EDGE('',*,*,#1723,.F.);
#2139=ORIENTED_EDGE('',*,*,#1724,.T.);
#2140=ORIENTED_EDGE('',*,*,#1725,.F.);
#2141=ORIENTED_EDGE('',*,*,#1724,.F.);
#2142=ORIENTED_EDGE('',*,*,#1726,.F.);
#2143=ORIENTED_EDGE('',*,*,#1727,.T.);
#2144=ORIENTED_EDGE('',*,*,#1728,.F.);
#2145=ORIENTED_EDGE('',*,*,#1727,.F.);
#2146=ORIENTED_EDGE('',*,*,#1729,.F.);
#2147=ORIENTED_EDGE('',*,*,#1730,.T.);
#2148=ORIENTED_EDGE('',*,*,#1731,.F.);
#2149=ORIENTED_EDGE('',*,*,#1730,.F.);
#2150=ORIENTED_EDGE('',*,*,#1732,.F.);
#2151=ORIENTED_EDGE('',*,*,#1733,.T.);
#2152=ORIENTED_EDGE('',*,*,#1734,.F.);
#2153=ORIENTED_EDGE('',*,*,#1735,.F.);
#2154=ORIENTED_EDGE('',*,*,#1736,.F.);
#2155=ORIENTED_EDGE('',*,*,#1737,.F.);
#2156=ORIENTED_EDGE('',*,*,#1738,.F.);
#2157=ORIENTED_EDGE('',*,*,#1739,.F.);
#2158=ORIENTED_EDGE('',*,*,#1740,.F.);
#2159=ORIENTED_EDGE('',*,*,#1739,.T.);
#2160=ORIENTED_EDGE('',*,*,#1741,.F.);
#2161=ORIENTED_EDGE('',*,*,#1733,.F.);
#2162=ORIENTED_EDGE('',*,*,#1740,.T.);
#2163=ORIENTED_EDGE('',*,*,#1732,.T.);
#2164=ORIENTED_EDGE('',*,*,#1742,.F.);
#2165=ORIENTED_EDGE('',*,*,#1736,.T.);
#2166=ORIENTED_EDGE('',*,*,#1729,.T.);
#2167=ORIENTED_EDGE('',*,*,#1737,.T.);
#2168=ORIENTED_EDGE('',*,*,#1742,.T.);
#2169=ORIENTED_EDGE('',*,*,#1735,.T.);
#2170=ORIENTED_EDGE('',*,*,#1743,.T.);
#2171=ORIENTED_EDGE('',*,*,#1744,.T.);
#2172=ORIENTED_EDGE('',*,*,#1745,.T.);
#2173=ORIENTED_EDGE('',*,*,#1746,.T.);
#2174=ORIENTED_EDGE('',*,*,#1747,.T.);
#2175=ORIENTED_EDGE('',*,*,#1725,.T.);
#2176=ORIENTED_EDGE('',*,*,#1728,.T.);
#2177=ORIENTED_EDGE('',*,*,#1748,.T.);
#2178=ORIENTED_EDGE('',*,*,#1749,.T.);
#2179=ORIENTED_EDGE('',*,*,#1743,.F.);
#2180=ORIENTED_EDGE('',*,*,#1734,.T.);
#2181=ORIENTED_EDGE('',*,*,#1741,.T.);
#2182=ORIENTED_EDGE('',*,*,#1738,.T.);
#2183=ORIENTED_EDGE('',*,*,#1747,.F.);
#2184=ORIENTED_EDGE('',*,*,#1750,.F.);
#2185=ORIENTED_EDGE('',*,*,#1731,.T.);
#2186=ORIENTED_EDGE('',*,*,#1751,.T.);
#2187=ORIENTED_EDGE('',*,*,#1750,.T.);
#2188=ORIENTED_EDGE('',*,*,#1746,.F.);
#2189=ORIENTED_EDGE('',*,*,#1752,.F.);
#2190=ORIENTED_EDGE('',*,*,#1753,.T.);
#2191=ORIENTED_EDGE('',*,*,#1752,.T.);
#2192=ORIENTED_EDGE('',*,*,#1745,.F.);
#2193=ORIENTED_EDGE('',*,*,#1754,.F.);
#2194=ORIENTED_EDGE('',*,*,#1755,.T.);
#2195=ORIENTED_EDGE('',*,*,#1754,.T.);
#2196=ORIENTED_EDGE('',*,*,#1744,.F.);
#2197=ORIENTED_EDGE('',*,*,#1749,.F.);
#2198=ORIENTED_EDGE('',*,*,#1755,.F.);
#2199=ORIENTED_EDGE('',*,*,#1748,.F.);
#2200=ORIENTED_EDGE('',*,*,#1751,.F.);
#2201=ORIENTED_EDGE('',*,*,#1753,.F.);
#2202=ORIENTED_EDGE('',*,*,#1723,.T.);
#2203=ORIENTED_EDGE('',*,*,#1726,.T.);
#2204=ORIENTED_EDGE('',*,*,#1756,.F.);
#2205=ORIENTED_EDGE('',*,*,#1757,.T.);
#2206=ORIENTED_EDGE('',*,*,#1758,.F.);
#2207=ORIENTED_EDGE('',*,*,#1759,.F.);
#2208=ORIENTED_EDGE('',*,*,#1760,.F.);
#2209=ORIENTED_EDGE('',*,*,#1761,.T.);
#2210=ORIENTED_EDGE('',*,*,#1762,.F.);
#2211=ORIENTED_EDGE('',*,*,#1757,.F.);
#2212=ORIENTED_EDGE('',*,*,#1763,.F.);
#2213=ORIENTED_EDGE('',*,*,#1764,.T.);
#2214=ORIENTED_EDGE('',*,*,#1765,.F.);
#2215=ORIENTED_EDGE('',*,*,#1761,.F.);
#2216=ORIENTED_EDGE('',*,*,#1766,.F.);
#2217=ORIENTED_EDGE('',*,*,#1767,.T.);
#2218=ORIENTED_EDGE('',*,*,#1768,.F.);
#2219=ORIENTED_EDGE('',*,*,#1764,.F.);
#2220=ORIENTED_EDGE('',*,*,#1769,.F.);
#2221=ORIENTED_EDGE('',*,*,#1770,.T.);
#2222=ORIENTED_EDGE('',*,*,#1771,.F.);
#2223=ORIENTED_EDGE('',*,*,#1767,.F.);
#2224=ORIENTED_EDGE('',*,*,#1772,.F.);
#2225=ORIENTED_EDGE('',*,*,#1773,.T.);
#2226=ORIENTED_EDGE('',*,*,#1774,.F.);
#2227=ORIENTED_EDGE('',*,*,#1770,.F.);
#2228=ORIENTED_EDGE('',*,*,#1775,.F.);
#2229=ORIENTED_EDGE('',*,*,#1776,.T.);
#2230=ORIENTED_EDGE('',*,*,#1777,.F.);
#2231=ORIENTED_EDGE('',*,*,#1773,.F.);
#2232=ORIENTED_EDGE('',*,*,#1778,.F.);
#2233=ORIENTED_EDGE('',*,*,#1779,.T.);
#2234=ORIENTED_EDGE('',*,*,#1780,.F.);
#2235=ORIENTED_EDGE('',*,*,#1776,.F.);
#2236=ORIENTED_EDGE('',*,*,#1781,.F.);
#2237=ORIENTED_EDGE('',*,*,#1782,.F.);
#2238=ORIENTED_EDGE('',*,*,#1783,.F.);
#2239=ORIENTED_EDGE('',*,*,#1779,.F.);
#2240=ORIENTED_EDGE('',*,*,#1784,.F.);
#2241=ORIENTED_EDGE('',*,*,#1785,.T.);
#2242=ORIENTED_EDGE('',*,*,#1786,.F.);
#2243=ORIENTED_EDGE('',*,*,#1787,.F.);
#2244=ORIENTED_EDGE('',*,*,#1788,.F.);
#2245=ORIENTED_EDGE('',*,*,#1789,.T.);
#2246=ORIENTED_EDGE('',*,*,#1790,.F.);
#2247=ORIENTED_EDGE('',*,*,#1785,.F.);
#2248=ORIENTED_EDGE('',*,*,#1791,.F.);
#2249=ORIENTED_EDGE('',*,*,#1792,.T.);
#2250=ORIENTED_EDGE('',*,*,#1793,.F.);
#2251=ORIENTED_EDGE('',*,*,#1789,.F.);
#2252=ORIENTED_EDGE('',*,*,#1794,.F.);
#2253=ORIENTED_EDGE('',*,*,#1795,.T.);
#2254=ORIENTED_EDGE('',*,*,#1796,.F.);
#2255=ORIENTED_EDGE('',*,*,#1792,.F.);
#2256=ORIENTED_EDGE('',*,*,#1797,.F.);
#2257=ORIENTED_EDGE('',*,*,#1798,.T.);
#2258=ORIENTED_EDGE('',*,*,#1799,.F.);
#2259=ORIENTED_EDGE('',*,*,#1795,.F.);
#2260=ORIENTED_EDGE('',*,*,#1800,.F.);
#2261=ORIENTED_EDGE('',*,*,#1801,.T.);
#2262=ORIENTED_EDGE('',*,*,#1802,.F.);
#2263=ORIENTED_EDGE('',*,*,#1798,.F.);
#2264=ORIENTED_EDGE('',*,*,#1803,.F.);
#2265=ORIENTED_EDGE('',*,*,#1804,.T.);
#2266=ORIENTED_EDGE('',*,*,#1805,.F.);
#2267=ORIENTED_EDGE('',*,*,#1801,.F.);
#2268=ORIENTED_EDGE('',*,*,#1806,.F.);
#2269=ORIENTED_EDGE('',*,*,#1807,.T.);
#2270=ORIENTED_EDGE('',*,*,#1808,.F.);
#2271=ORIENTED_EDGE('',*,*,#1804,.F.);
#2272=ORIENTED_EDGE('',*,*,#1809,.F.);
#2273=ORIENTED_EDGE('',*,*,#1810,.F.);
#2274=ORIENTED_EDGE('',*,*,#1811,.F.);
#2275=ORIENTED_EDGE('',*,*,#1807,.F.);
#2276=ORIENTED_EDGE('',*,*,#1812,.F.);
#2277=ORIENTED_EDGE('',*,*,#1813,.T.);
#2278=ORIENTED_EDGE('',*,*,#1814,.F.);
#2279=ORIENTED_EDGE('',*,*,#1815,.F.);
#2280=ORIENTED_EDGE('',*,*,#1816,.F.);
#2281=ORIENTED_EDGE('',*,*,#1817,.T.);
#2282=ORIENTED_EDGE('',*,*,#1818,.F.);
#2283=ORIENTED_EDGE('',*,*,#1813,.F.);
#2284=ORIENTED_EDGE('',*,*,#1819,.F.);
#2285=ORIENTED_EDGE('',*,*,#1820,.T.);
#2286=ORIENTED_EDGE('',*,*,#1821,.F.);
#2287=ORIENTED_EDGE('',*,*,#1817,.F.);
#2288=ORIENTED_EDGE('',*,*,#1822,.F.);
#2289=ORIENTED_EDGE('',*,*,#1823,.T.);
#2290=ORIENTED_EDGE('',*,*,#1824,.F.);
#2291=ORIENTED_EDGE('',*,*,#1820,.F.);
#2292=ORIENTED_EDGE('',*,*,#1825,.F.);
#2293=ORIENTED_EDGE('',*,*,#1826,.T.);
#2294=ORIENTED_EDGE('',*,*,#1827,.F.);
#2295=ORIENTED_EDGE('',*,*,#1823,.F.);
#2296=ORIENTED_EDGE('',*,*,#1828,.F.);
#2297=ORIENTED_EDGE('',*,*,#1829,.T.);
#2298=ORIENTED_EDGE('',*,*,#1830,.F.);
#2299=ORIENTED_EDGE('',*,*,#1826,.F.);
#2300=ORIENTED_EDGE('',*,*,#1831,.F.);
#2301=ORIENTED_EDGE('',*,*,#1832,.T.);
#2302=ORIENTED_EDGE('',*,*,#1833,.F.);
#2303=ORIENTED_EDGE('',*,*,#1829,.F.);
#2304=ORIENTED_EDGE('',*,*,#1834,.F.);
#2305=ORIENTED_EDGE('',*,*,#1835,.T.);
#2306=ORIENTED_EDGE('',*,*,#1836,.F.);
#2307=ORIENTED_EDGE('',*,*,#1832,.F.);
#2308=ORIENTED_EDGE('',*,*,#1837,.F.);
#2309=ORIENTED_EDGE('',*,*,#1838,.F.);
#2310=ORIENTED_EDGE('',*,*,#1839,.F.);
#2311=ORIENTED_EDGE('',*,*,#1835,.F.);
#2312=ORIENTED_EDGE('',*,*,#1840,.F.);
#2313=ORIENTED_EDGE('',*,*,#1841,.T.);
#2314=ORIENTED_EDGE('',*,*,#1842,.F.);
#2315=ORIENTED_EDGE('',*,*,#1843,.F.);
#2316=ORIENTED_EDGE('',*,*,#1844,.F.);
#2317=ORIENTED_EDGE('',*,*,#1845,.T.);
#2318=ORIENTED_EDGE('',*,*,#1846,.F.);
#2319=ORIENTED_EDGE('',*,*,#1841,.F.);
#2320=ORIENTED_EDGE('',*,*,#1847,.F.);
#2321=ORIENTED_EDGE('',*,*,#1848,.T.);
#2322=ORIENTED_EDGE('',*,*,#1849,.F.);
#2323=ORIENTED_EDGE('',*,*,#1845,.F.);
#2324=ORIENTED_EDGE('',*,*,#1850,.F.);
#2325=ORIENTED_EDGE('',*,*,#1851,.T.);
#2326=ORIENTED_EDGE('',*,*,#1852,.F.);
#2327=ORIENTED_EDGE('',*,*,#1848,.F.);
#2328=ORIENTED_EDGE('',*,*,#1853,.F.);
#2329=ORIENTED_EDGE('',*,*,#1854,.T.);
#2330=ORIENTED_EDGE('',*,*,#1855,.F.);
#2331=ORIENTED_EDGE('',*,*,#1851,.F.);
#2332=ORIENTED_EDGE('',*,*,#1856,.F.);
#2333=ORIENTED_EDGE('',*,*,#1857,.T.);
#2334=ORIENTED_EDGE('',*,*,#1858,.F.);
#2335=ORIENTED_EDGE('',*,*,#1854,.F.);
#2336=ORIENTED_EDGE('',*,*,#1859,.F.);
#2337=ORIENTED_EDGE('',*,*,#1860,.T.);
#2338=ORIENTED_EDGE('',*,*,#1861,.F.);
#2339=ORIENTED_EDGE('',*,*,#1857,.F.);
#2340=ORIENTED_EDGE('',*,*,#1862,.F.);
#2341=ORIENTED_EDGE('',*,*,#1863,.T.);
#2342=ORIENTED_EDGE('',*,*,#1864,.F.);
#2343=ORIENTED_EDGE('',*,*,#1860,.F.);
#2344=ORIENTED_EDGE('',*,*,#1865,.F.);
#2345=ORIENTED_EDGE('',*,*,#1866,.F.);
#2346=ORIENTED_EDGE('',*,*,#1867,.F.);
#2347=ORIENTED_EDGE('',*,*,#1863,.F.);
#2348=ORIENTED_EDGE('',*,*,#1868,.F.);
#2349=ORIENTED_EDGE('',*,*,#1869,.T.);
#2350=ORIENTED_EDGE('',*,*,#1870,.F.);
#2351=ORIENTED_EDGE('',*,*,#1869,.F.);
#2352=ORIENTED_EDGE('',*,*,#1782,.T.);
#2353=ORIENTED_EDGE('',*,*,#1871,.T.);
#2354=ORIENTED_EDGE('',*,*,#1872,.T.);
#2355=ORIENTED_EDGE('',*,*,#1873,.F.);
#2356=ORIENTED_EDGE('',*,*,#1759,.T.);
#2357=ORIENTED_EDGE('',*,*,#1874,.F.);
#2358=ORIENTED_EDGE('',*,*,#1875,.F.);
#2359=ORIENTED_EDGE('',*,*,#1876,.T.);
#2360=ORIENTED_EDGE('',*,*,#1810,.T.);
#2361=ORIENTED_EDGE('',*,*,#1877,.T.);
#2362=ORIENTED_EDGE('',*,*,#1875,.T.);
#2363=ORIENTED_EDGE('',*,*,#1878,.F.);
#2364=ORIENTED_EDGE('',*,*,#1787,.T.);
#2365=ORIENTED_EDGE('',*,*,#1879,.F.);
#2366=ORIENTED_EDGE('',*,*,#1880,.F.);
#2367=ORIENTED_EDGE('',*,*,#1881,.T.);
#2368=ORIENTED_EDGE('',*,*,#1838,.T.);
#2369=ORIENTED_EDGE('',*,*,#1882,.T.);
#2370=ORIENTED_EDGE('',*,*,#1880,.T.);
#2371=ORIENTED_EDGE('',*,*,#1883,.F.);
#2372=ORIENTED_EDGE('',*,*,#1815,.T.);
#2373=ORIENTED_EDGE('',*,*,#1884,.F.);
#2374=ORIENTED_EDGE('',*,*,#1885,.F.);
#2375=ORIENTED_EDGE('',*,*,#1886,.T.);
#2376=ORIENTED_EDGE('',*,*,#1866,.T.);
#2377=ORIENTED_EDGE('',*,*,#1887,.T.);
#2378=ORIENTED_EDGE('',*,*,#1885,.T.);
#2379=ORIENTED_EDGE('',*,*,#1888,.F.);
#2380=ORIENTED_EDGE('',*,*,#1843,.T.);
#2381=ORIENTED_EDGE('',*,*,#1889,.F.);
#2382=ORIENTED_EDGE('',*,*,#1872,.F.);
#2383=ORIENTED_EDGE('',*,*,#1890,.T.);
#2384=ORIENTED_EDGE('',*,*,#1758,.T.);
#2385=ORIENTED_EDGE('',*,*,#1762,.T.);
#2386=ORIENTED_EDGE('',*,*,#1765,.T.);
#2387=ORIENTED_EDGE('',*,*,#1768,.T.);
#2388=ORIENTED_EDGE('',*,*,#1771,.T.);
#2389=ORIENTED_EDGE('',*,*,#1774,.T.);
#2390=ORIENTED_EDGE('',*,*,#1777,.T.);
#2391=ORIENTED_EDGE('',*,*,#1780,.T.);
#2392=ORIENTED_EDGE('',*,*,#1783,.T.);
#2393=ORIENTED_EDGE('',*,*,#1873,.T.);
#2394=ORIENTED_EDGE('',*,*,#1889,.T.);
#2395=ORIENTED_EDGE('',*,*,#1842,.T.);
#2396=ORIENTED_EDGE('',*,*,#1846,.T.);
#2397=ORIENTED_EDGE('',*,*,#1849,.T.);
#2398=ORIENTED_EDGE('',*,*,#1852,.T.);
#2399=ORIENTED_EDGE('',*,*,#1855,.T.);
#2400=ORIENTED_EDGE('',*,*,#1858,.T.);
#2401=ORIENTED_EDGE('',*,*,#1861,.T.);
#2402=ORIENTED_EDGE('',*,*,#1864,.T.);
#2403=ORIENTED_EDGE('',*,*,#1867,.T.);
#2404=ORIENTED_EDGE('',*,*,#1888,.T.);
#2405=ORIENTED_EDGE('',*,*,#1884,.T.);
#2406=ORIENTED_EDGE('',*,*,#1814,.T.);
#2407=ORIENTED_EDGE('',*,*,#1818,.T.);
#2408=ORIENTED_EDGE('',*,*,#1821,.T.);
#2409=ORIENTED_EDGE('',*,*,#1824,.T.);
#2410=ORIENTED_EDGE('',*,*,#1827,.T.);
#2411=ORIENTED_EDGE('',*,*,#1830,.T.);
#2412=ORIENTED_EDGE('',*,*,#1833,.T.);
#2413=ORIENTED_EDGE('',*,*,#1836,.T.);
#2414=ORIENTED_EDGE('',*,*,#1839,.T.);
#2415=ORIENTED_EDGE('',*,*,#1883,.T.);
#2416=ORIENTED_EDGE('',*,*,#1879,.T.);
#2417=ORIENTED_EDGE('',*,*,#1786,.T.);
#2418=ORIENTED_EDGE('',*,*,#1790,.T.);
#2419=ORIENTED_EDGE('',*,*,#1793,.T.);
#2420=ORIENTED_EDGE('',*,*,#1796,.T.);
#2421=ORIENTED_EDGE('',*,*,#1799,.T.);
#2422=ORIENTED_EDGE('',*,*,#1802,.T.);
#2423=ORIENTED_EDGE('',*,*,#1805,.T.);
#2424=ORIENTED_EDGE('',*,*,#1808,.T.);
#2425=ORIENTED_EDGE('',*,*,#1811,.T.);
#2426=ORIENTED_EDGE('',*,*,#1878,.T.);
#2427=ORIENTED_EDGE('',*,*,#1874,.T.);
#2428=ORIENTED_EDGE('',*,*,#1870,.T.);
#2429=ORIENTED_EDGE('',*,*,#1756,.T.);
#2430=ORIENTED_EDGE('',*,*,#1876,.F.);
#2431=ORIENTED_EDGE('',*,*,#1877,.F.);
#2432=ORIENTED_EDGE('',*,*,#1809,.T.);
#2433=ORIENTED_EDGE('',*,*,#1806,.T.);
#2434=ORIENTED_EDGE('',*,*,#1803,.T.);
#2435=ORIENTED_EDGE('',*,*,#1800,.T.);
#2436=ORIENTED_EDGE('',*,*,#1797,.T.);
#2437=ORIENTED_EDGE('',*,*,#1794,.T.);
#2438=ORIENTED_EDGE('',*,*,#1791,.T.);
#2439=ORIENTED_EDGE('',*,*,#1788,.T.);
#2440=ORIENTED_EDGE('',*,*,#1784,.T.);
#2441=ORIENTED_EDGE('',*,*,#1881,.F.);
#2442=ORIENTED_EDGE('',*,*,#1882,.F.);
#2443=ORIENTED_EDGE('',*,*,#1837,.T.);
#2444=ORIENTED_EDGE('',*,*,#1834,.T.);
#2445=ORIENTED_EDGE('',*,*,#1831,.T.);
#2446=ORIENTED_EDGE('',*,*,#1828,.T.);
#2447=ORIENTED_EDGE('',*,*,#1825,.T.);
#2448=ORIENTED_EDGE('',*,*,#1822,.T.);
#2449=ORIENTED_EDGE('',*,*,#1819,.T.);
#2450=ORIENTED_EDGE('',*,*,#1816,.T.);
#2451=ORIENTED_EDGE('',*,*,#1812,.T.);
#2452=ORIENTED_EDGE('',*,*,#1886,.F.);
#2453=ORIENTED_EDGE('',*,*,#1887,.F.);
#2454=ORIENTED_EDGE('',*,*,#1865,.T.);
#2455=ORIENTED_EDGE('',*,*,#1862,.T.);
#2456=ORIENTED_EDGE('',*,*,#1859,.T.);
#2457=ORIENTED_EDGE('',*,*,#1856,.T.);
#2458=ORIENTED_EDGE('',*,*,#1853,.T.);
#2459=ORIENTED_EDGE('',*,*,#1850,.T.);
#2460=ORIENTED_EDGE('',*,*,#1847,.T.);
#2461=ORIENTED_EDGE('',*,*,#1844,.T.);
#2462=ORIENTED_EDGE('',*,*,#1840,.T.);
#2463=ORIENTED_EDGE('',*,*,#1890,.F.);
#2464=ORIENTED_EDGE('',*,*,#1871,.F.);
#2465=ORIENTED_EDGE('',*,*,#1781,.T.);
#2466=ORIENTED_EDGE('',*,*,#1778,.T.);
#2467=ORIENTED_EDGE('',*,*,#1775,.T.);
#2468=ORIENTED_EDGE('',*,*,#1772,.T.);
#2469=ORIENTED_EDGE('',*,*,#1769,.T.);
#2470=ORIENTED_EDGE('',*,*,#1766,.T.);
#2471=ORIENTED_EDGE('',*,*,#1763,.T.);
#2472=ORIENTED_EDGE('',*,*,#1760,.T.);
#2473=ORIENTED_EDGE('',*,*,#1868,.T.);
#2474=ORIENTED_EDGE('',*,*,#1891,.F.);
#2475=ORIENTED_EDGE('',*,*,#1892,.F.);
#2476=ORIENTED_EDGE('',*,*,#1893,.F.);
#2477=ORIENTED_EDGE('',*,*,#1894,.F.);
#2478=ORIENTED_EDGE('',*,*,#1893,.T.);
#2479=ORIENTED_EDGE('',*,*,#1895,.T.);
#2480=ORIENTED_EDGE('',*,*,#1896,.F.);
#2481=ORIENTED_EDGE('',*,*,#1897,.F.);
#2482=ORIENTED_EDGE('',*,*,#1898,.T.);
#2483=ORIENTED_EDGE('',*,*,#1899,.T.);
#2484=ORIENTED_EDGE('',*,*,#1900,.T.);
#2485=ORIENTED_EDGE('',*,*,#1896,.T.);
#2486=ORIENTED_EDGE('',*,*,#1901,.T.);
#2487=ORIENTED_EDGE('',*,*,#1898,.F.);
#2488=ORIENTED_EDGE('',*,*,#1895,.F.);
#2489=ORIENTED_EDGE('',*,*,#1892,.T.);
#2490=ORIENTED_EDGE('',*,*,#1902,.F.);
#2491=ORIENTED_EDGE('',*,*,#1903,.F.);
#2492=ORIENTED_EDGE('',*,*,#1904,.T.);
#2493=ORIENTED_EDGE('',*,*,#1905,.F.);
#2494=ORIENTED_EDGE('',*,*,#1906,.T.);
#2495=ORIENTED_EDGE('',*,*,#1907,.T.);
#2496=ORIENTED_EDGE('',*,*,#1908,.T.);
#2497=ORIENTED_EDGE('',*,*,#1909,.T.);
#2498=ORIENTED_EDGE('',*,*,#1910,.T.);
#2499=ORIENTED_EDGE('',*,*,#1899,.F.);
#2500=ORIENTED_EDGE('',*,*,#1908,.F.);
#2501=ORIENTED_EDGE('',*,*,#1911,.F.);
#2502=ORIENTED_EDGE('',*,*,#1912,.F.);
#2503=ORIENTED_EDGE('',*,*,#1909,.F.);
#2504=ORIENTED_EDGE('',*,*,#1907,.F.);
#2505=ORIENTED_EDGE('',*,*,#1900,.F.);
#2506=ORIENTED_EDGE('',*,*,#1910,.F.);
#2507=ORIENTED_EDGE('',*,*,#1912,.T.);
#2508=ORIENTED_EDGE('',*,*,#1913,.F.);
#2509=ORIENTED_EDGE('',*,*,#1914,.F.);
#2510=ORIENTED_EDGE('',*,*,#1915,.T.);
#2511=ORIENTED_EDGE('',*,*,#1916,.F.);
#2512=ORIENTED_EDGE('',*,*,#1917,.T.);
#2513=ORIENTED_EDGE('',*,*,#1894,.T.);
#2514=ORIENTED_EDGE('',*,*,#1897,.T.);
#2515=ORIENTED_EDGE('',*,*,#1911,.T.);
#2516=ORIENTED_EDGE('',*,*,#1906,.F.);
#2517=ORIENTED_EDGE('',*,*,#1918,.F.);
#2518=ORIENTED_EDGE('',*,*,#1913,.T.);
#2519=ORIENTED_EDGE('',*,*,#1914,.T.);
#2520=ORIENTED_EDGE('',*,*,#1918,.T.);
#2521=ORIENTED_EDGE('',*,*,#1905,.T.);
#2522=ORIENTED_EDGE('',*,*,#1919,.T.);
#2523=ORIENTED_EDGE('',*,*,#1920,.T.);
#2524=ORIENTED_EDGE('',*,*,#1921,.T.);
#2525=ORIENTED_EDGE('',*,*,#1920,.F.);
#2526=ORIENTED_EDGE('',*,*,#1922,.F.);
#2527=ORIENTED_EDGE('',*,*,#1923,.T.);
#2528=ORIENTED_EDGE('',*,*,#1901,.F.);
#2529=ORIENTED_EDGE('',*,*,#1923,.F.);
#2530=ORIENTED_EDGE('',*,*,#1924,.F.);
#2531=ORIENTED_EDGE('',*,*,#1925,.F.);
#2532=ORIENTED_EDGE('',*,*,#1926,.F.);
#2533=ORIENTED_EDGE('',*,*,#1919,.F.);
#2534=ORIENTED_EDGE('',*,*,#1904,.F.);
#2535=ORIENTED_EDGE('',*,*,#1927,.F.);
#2536=ORIENTED_EDGE('',*,*,#1924,.T.);
#2537=ORIENTED_EDGE('',*,*,#1922,.T.);
#2538=ORIENTED_EDGE('',*,*,#1921,.F.);
#2539=ORIENTED_EDGE('',*,*,#1926,.T.);
#2540=ORIENTED_EDGE('',*,*,#1928,.F.);
#2541=ORIENTED_EDGE('',*,*,#1915,.F.);
#2542=ORIENTED_EDGE('',*,*,#1903,.T.);
#2543=ORIENTED_EDGE('',*,*,#1929,.T.);
#2544=ORIENTED_EDGE('',*,*,#1916,.T.);
#2545=ORIENTED_EDGE('',*,*,#1928,.T.);
#2546=ORIENTED_EDGE('',*,*,#1925,.T.);
#2547=ORIENTED_EDGE('',*,*,#1927,.T.);
#2548=ORIENTED_EDGE('',*,*,#1891,.T.);
#2549=ORIENTED_EDGE('',*,*,#1917,.F.);
#2550=ORIENTED_EDGE('',*,*,#1929,.F.);
#2551=ORIENTED_EDGE('',*,*,#1902,.T.);
#2552=ORIENTED_EDGE('',*,*,#1930,.T.);
#2553=ORIENTED_EDGE('',*,*,#1931,.T.);
#2554=ORIENTED_EDGE('',*,*,#1932,.T.);
#2555=ORIENTED_EDGE('',*,*,#1931,.F.);
#2556=ORIENTED_EDGE('',*,*,#1932,.F.);
#2557=ORIENTED_EDGE('',*,*,#1933,.T.);
#2558=ORIENTED_EDGE('',*,*,#1934,.T.);
#2559=ORIENTED_EDGE('',*,*,#1933,.F.);
#2560=ORIENTED_EDGE('',*,*,#1935,.T.);
#2561=ORIENTED_EDGE('',*,*,#1930,.F.);
#2562=ORIENTED_EDGE('',*,*,#1935,.F.);
#2563=ORIENTED_EDGE('',*,*,#1936,.T.);
#2564=ORIENTED_EDGE('',*,*,#1937,.T.);
#2565=ORIENTED_EDGE('',*,*,#1936,.F.);
#2566=ORIENTED_EDGE('',*,*,#1937,.F.);
#2567=ORIENTED_EDGE('',*,*,#1934,.F.);
#2568=ORIENTED_EDGE('',*,*,#1938,.T.);
#2569=ORIENTED_EDGE('',*,*,#1939,.T.);
#2570=ORIENTED_EDGE('',*,*,#1940,.T.);
#2571=ORIENTED_EDGE('',*,*,#1941,.F.);
#2572=ORIENTED_EDGE('',*,*,#1942,.T.);
#2573=ORIENTED_EDGE('',*,*,#1943,.T.);
#2574=ORIENTED_EDGE('',*,*,#1944,.T.);
#2575=ORIENTED_EDGE('',*,*,#1939,.F.);
#2576=ORIENTED_EDGE('',*,*,#1945,.T.);
#2577=ORIENTED_EDGE('',*,*,#1946,.T.);
#2578=ORIENTED_EDGE('',*,*,#1947,.T.);
#2579=ORIENTED_EDGE('',*,*,#1943,.F.);
#2580=ORIENTED_EDGE('',*,*,#1948,.T.);
#2581=ORIENTED_EDGE('',*,*,#1949,.T.);
#2582=ORIENTED_EDGE('',*,*,#1950,.T.);
#2583=ORIENTED_EDGE('',*,*,#1946,.F.);
#2584=ORIENTED_EDGE('',*,*,#1951,.T.);
#2585=ORIENTED_EDGE('',*,*,#1952,.T.);
#2586=ORIENTED_EDGE('',*,*,#1953,.T.);
#2587=ORIENTED_EDGE('',*,*,#1949,.F.);
#2588=ORIENTED_EDGE('',*,*,#1954,.T.);
#2589=ORIENTED_EDGE('',*,*,#1941,.T.);
#2590=ORIENTED_EDGE('',*,*,#1955,.T.);
#2591=ORIENTED_EDGE('',*,*,#1952,.F.);
#2592=ORIENTED_EDGE('',*,*,#1954,.F.);
#2593=ORIENTED_EDGE('',*,*,#1951,.F.);
#2594=ORIENTED_EDGE('',*,*,#1948,.F.);
#2595=ORIENTED_EDGE('',*,*,#1945,.F.);
#2596=ORIENTED_EDGE('',*,*,#1942,.F.);
#2597=ORIENTED_EDGE('',*,*,#1938,.F.);
#2598=ORIENTED_EDGE('',*,*,#1955,.F.);
#2599=ORIENTED_EDGE('',*,*,#1940,.F.);
#2600=ORIENTED_EDGE('',*,*,#1944,.F.);
#2601=ORIENTED_EDGE('',*,*,#1947,.F.);
#2602=ORIENTED_EDGE('',*,*,#1950,.F.);
#2603=ORIENTED_EDGE('',*,*,#1953,.F.);
#2604=ORIENTED_EDGE('',*,*,#1956,.F.);
#2605=ORIENTED_EDGE('',*,*,#1957,.F.);
#2606=ORIENTED_EDGE('',*,*,#1958,.F.);
#2607=ORIENTED_EDGE('',*,*,#1959,.T.);
#2608=ORIENTED_EDGE('',*,*,#1957,.T.);
#2609=ORIENTED_EDGE('',*,*,#1959,.F.);
#2610=ORIENTED_EDGE('',*,*,#1960,.F.);
#2611=ORIENTED_EDGE('',*,*,#1961,.T.);
#2612=ORIENTED_EDGE('',*,*,#1958,.T.);
#2613=ORIENTED_EDGE('',*,*,#1961,.F.);
#2614=ORIENTED_EDGE('',*,*,#1962,.F.);
#2615=ORIENTED_EDGE('',*,*,#1963,.T.);
#2616=ORIENTED_EDGE('',*,*,#1960,.T.);
#2617=ORIENTED_EDGE('',*,*,#1963,.F.);
#2618=ORIENTED_EDGE('',*,*,#1962,.T.);
#2619=ORIENTED_EDGE('',*,*,#1964,.F.);
#2620=ORIENTED_EDGE('',*,*,#1965,.F.);
#2621=ORIENTED_EDGE('',*,*,#1966,.T.);
#2622=ORIENTED_EDGE('',*,*,#1964,.T.);
#2623=ORIENTED_EDGE('',*,*,#1966,.F.);
#2624=ORIENTED_EDGE('',*,*,#1956,.T.);
#2625=ORIENTED_EDGE('',*,*,#1967,.T.);
#2626=ORIENTED_EDGE('',*,*,#1965,.T.);
#2627=ORIENTED_EDGE('',*,*,#1967,.F.);
#2628=ORIENTED_EDGE('',*,*,#1968,.F.);
#2629=ORIENTED_EDGE('',*,*,#1969,.T.);
#2630=ORIENTED_EDGE('',*,*,#1970,.F.);
#2631=ORIENTED_EDGE('',*,*,#1969,.F.);
#2632=ORIENTED_EDGE('',*,*,#1971,.F.);
#2633=ORIENTED_EDGE('',*,*,#1972,.T.);
#2634=ORIENTED_EDGE('',*,*,#1973,.F.);
#2635=ORIENTED_EDGE('',*,*,#1972,.F.);
#2636=ORIENTED_EDGE('',*,*,#1974,.F.);
#2637=ORIENTED_EDGE('',*,*,#1975,.F.);
#2638=ORIENTED_EDGE('',*,*,#1976,.F.);
#2639=ORIENTED_EDGE('',*,*,#1977,.T.);
#2640=ORIENTED_EDGE('',*,*,#1974,.T.);
#2641=ORIENTED_EDGE('',*,*,#1978,.F.);
#2642=ORIENTED_EDGE('',*,*,#1979,.F.);
#2643=ORIENTED_EDGE('',*,*,#1980,.F.);
#2644=ORIENTED_EDGE('',*,*,#1977,.F.);
#2645=ORIENTED_EDGE('',*,*,#1981,.T.);
#2646=ORIENTED_EDGE('',*,*,#1982,.F.);
#2647=ORIENTED_EDGE('',*,*,#1978,.T.);
#2648=ORIENTED_EDGE('',*,*,#1968,.T.);
#2649=ORIENTED_EDGE('',*,*,#1971,.T.);
#2650=ORIENTED_EDGE('',*,*,#1976,.T.);
#2651=ORIENTED_EDGE('',*,*,#1983,.F.);
#2652=ORIENTED_EDGE('',*,*,#1984,.F.);
#2653=ORIENTED_EDGE('',*,*,#1981,.F.);
#2654=ORIENTED_EDGE('',*,*,#1979,.T.);
#2655=ORIENTED_EDGE('',*,*,#1982,.T.);
#2656=ORIENTED_EDGE('',*,*,#1984,.T.);
#2657=ORIENTED_EDGE('',*,*,#1985,.F.);
#2658=ORIENTED_EDGE('',*,*,#1980,.T.);
#2659=ORIENTED_EDGE('',*,*,#1985,.T.);
#2660=ORIENTED_EDGE('',*,*,#1983,.T.);
#2661=ORIENTED_EDGE('',*,*,#1975,.T.);
#2662=ORIENTED_EDGE('',*,*,#1970,.T.);
#2663=ORIENTED_EDGE('',*,*,#1973,.T.);
#2664=ORIENTED_EDGE('',*,*,#1986,.F.);
#2665=ORIENTED_EDGE('',*,*,#1987,.T.);
#2666=ORIENTED_EDGE('',*,*,#1988,.F.);
#2667=ORIENTED_EDGE('',*,*,#1987,.F.);
#2668=ORIENTED_EDGE('',*,*,#1989,.F.);
#2669=ORIENTED_EDGE('',*,*,#1990,.T.);
#2670=ORIENTED_EDGE('',*,*,#1986,.T.);
#2671=ORIENTED_EDGE('',*,*,#1990,.F.);
#2672=ORIENTED_EDGE('',*,*,#1989,.T.);
#2673=ORIENTED_EDGE('',*,*,#1991,.F.);
#2674=ORIENTED_EDGE('',*,*,#1992,.T.);
#2675=ORIENTED_EDGE('',*,*,#1993,.F.);
#2676=ORIENTED_EDGE('',*,*,#1994,.F.);
#2677=ORIENTED_EDGE('',*,*,#1995,.F.);
#2678=ORIENTED_EDGE('',*,*,#1996,.F.);
#2679=ORIENTED_EDGE('',*,*,#1997,.F.);
#2680=ORIENTED_EDGE('',*,*,#1998,.F.);
#2681=ORIENTED_EDGE('',*,*,#1992,.F.);
#2682=ORIENTED_EDGE('',*,*,#1997,.T.);
#2683=ORIENTED_EDGE('',*,*,#1999,.F.);
#2684=ORIENTED_EDGE('',*,*,#2000,.T.);
#2685=ORIENTED_EDGE('',*,*,#2001,.T.);
#2686=ORIENTED_EDGE('',*,*,#1996,.T.);
#2687=ORIENTED_EDGE('',*,*,#2002,.F.);
#2688=ORIENTED_EDGE('',*,*,#2003,.T.);
#2689=ORIENTED_EDGE('',*,*,#1999,.T.);
#2690=ORIENTED_EDGE('',*,*,#1995,.T.);
#2691=ORIENTED_EDGE('',*,*,#2004,.F.);
#2692=ORIENTED_EDGE('',*,*,#2005,.T.);
#2693=ORIENTED_EDGE('',*,*,#2002,.T.);
#2694=ORIENTED_EDGE('',*,*,#1994,.T.);
#2695=ORIENTED_EDGE('',*,*,#2006,.F.);
#2696=ORIENTED_EDGE('',*,*,#2007,.T.);
#2697=ORIENTED_EDGE('',*,*,#2004,.T.);
#2698=ORIENTED_EDGE('',*,*,#1993,.T.);
#2699=ORIENTED_EDGE('',*,*,#2008,.F.);
#2700=ORIENTED_EDGE('',*,*,#2009,.T.);
#2701=ORIENTED_EDGE('',*,*,#2006,.T.);
#2702=ORIENTED_EDGE('',*,*,#1998,.T.);
#2703=ORIENTED_EDGE('',*,*,#2001,.F.);
#2704=ORIENTED_EDGE('',*,*,#2010,.T.);
#2705=ORIENTED_EDGE('',*,*,#2008,.T.);
#2706=ORIENTED_EDGE('',*,*,#1991,.T.);
#2707=ORIENTED_EDGE('',*,*,#2005,.F.);
#2708=ORIENTED_EDGE('',*,*,#2007,.F.);
#2709=ORIENTED_EDGE('',*,*,#2009,.F.);
#2710=ORIENTED_EDGE('',*,*,#2010,.F.);
#2711=ORIENTED_EDGE('',*,*,#2000,.F.);
#2712=ORIENTED_EDGE('',*,*,#2003,.F.);
#2713=ORIENTED_EDGE('',*,*,#1988,.T.);
#2714=ORIENTED_EDGE('',*,*,#2011,.F.);
#2715=ORIENTED_EDGE('',*,*,#2012,.T.);
#2716=ORIENTED_EDGE('',*,*,#2013,.F.);
#2717=ORIENTED_EDGE('',*,*,#2012,.F.);
#2718=ORIENTED_EDGE('',*,*,#2014,.F.);
#2719=ORIENTED_EDGE('',*,*,#2015,.T.);
#2720=ORIENTED_EDGE('',*,*,#2016,.F.);
#2721=ORIENTED_EDGE('',*,*,#2015,.F.);
#2722=ORIENTED_EDGE('',*,*,#2017,.F.);
#2723=ORIENTED_EDGE('',*,*,#2018,.T.);
#2724=ORIENTED_EDGE('',*,*,#2019,.F.);
#2725=ORIENTED_EDGE('',*,*,#2018,.F.);
#2726=ORIENTED_EDGE('',*,*,#2020,.F.);
#2727=ORIENTED_EDGE('',*,*,#2021,.T.);
#2728=ORIENTED_EDGE('',*,*,#2022,.F.);
#2729=ORIENTED_EDGE('',*,*,#2021,.F.);
#2730=ORIENTED_EDGE('',*,*,#2023,.F.);
#2731=ORIENTED_EDGE('',*,*,#2024,.T.);
#2732=ORIENTED_EDGE('',*,*,#2025,.F.);
#2733=ORIENTED_EDGE('',*,*,#2024,.F.);
#2734=ORIENTED_EDGE('',*,*,#2026,.F.);
#2735=ORIENTED_EDGE('',*,*,#2027,.F.);
#2736=ORIENTED_EDGE('',*,*,#2028,.F.);
#2737=ORIENTED_EDGE('',*,*,#2029,.F.);
#2738=ORIENTED_EDGE('',*,*,#2030,.F.);
#2739=ORIENTED_EDGE('',*,*,#2031,.T.);
#2740=ORIENTED_EDGE('',*,*,#2032,.F.);
#2741=ORIENTED_EDGE('',*,*,#2033,.F.);
#2742=ORIENTED_EDGE('',*,*,#2034,.F.);
#2743=ORIENTED_EDGE('',*,*,#2035,.F.);
#2744=ORIENTED_EDGE('',*,*,#2033,.T.);
#2745=ORIENTED_EDGE('',*,*,#2036,.F.);
#2746=ORIENTED_EDGE('',*,*,#2037,.F.);
#2747=ORIENTED_EDGE('',*,*,#2028,.T.);
#2748=ORIENTED_EDGE('',*,*,#2038,.F.);
#2749=ORIENTED_EDGE('',*,*,#2039,.F.);
#2750=ORIENTED_EDGE('',*,*,#2040,.F.);
#2751=ORIENTED_EDGE('',*,*,#2039,.T.);
#2752=ORIENTED_EDGE('',*,*,#2041,.F.);
#2753=ORIENTED_EDGE('',*,*,#2031,.F.);
#2754=ORIENTED_EDGE('',*,*,#2034,.T.);
#2755=ORIENTED_EDGE('',*,*,#2042,.F.);
#2756=ORIENTED_EDGE('',*,*,#2043,.F.);
#2757=ORIENTED_EDGE('',*,*,#2044,.F.);
#2758=ORIENTED_EDGE('',*,*,#2036,.T.);
#2759=ORIENTED_EDGE('',*,*,#2032,.T.);
#2760=ORIENTED_EDGE('',*,*,#2041,.T.);
#2761=ORIENTED_EDGE('',*,*,#2038,.T.);
#2762=ORIENTED_EDGE('',*,*,#2027,.T.);
#2763=ORIENTED_EDGE('',*,*,#2045,.T.);
#2764=ORIENTED_EDGE('',*,*,#2046,.T.);
#2765=ORIENTED_EDGE('',*,*,#2042,.T.);
#2766=ORIENTED_EDGE('',*,*,#2025,.T.);
#2767=ORIENTED_EDGE('',*,*,#2022,.T.);
#2768=ORIENTED_EDGE('',*,*,#2019,.T.);
#2769=ORIENTED_EDGE('',*,*,#2016,.T.);
#2770=ORIENTED_EDGE('',*,*,#2013,.T.);
#2771=ORIENTED_EDGE('',*,*,#2026,.T.);
#2772=ORIENTED_EDGE('',*,*,#2047,.F.);
#2773=ORIENTED_EDGE('',*,*,#2048,.F.);
#2774=ORIENTED_EDGE('',*,*,#2045,.F.);
#2775=ORIENTED_EDGE('',*,*,#2043,.T.);
#2776=ORIENTED_EDGE('',*,*,#2046,.F.);
#2777=ORIENTED_EDGE('',*,*,#2048,.T.);
#2778=ORIENTED_EDGE('',*,*,#2049,.T.);
#2779=ORIENTED_EDGE('',*,*,#2044,.T.);
#2780=ORIENTED_EDGE('',*,*,#2049,.F.);
#2781=ORIENTED_EDGE('',*,*,#2047,.T.);
#2782=ORIENTED_EDGE('',*,*,#2029,.T.);
#2783=ORIENTED_EDGE('',*,*,#2037,.T.);
#2784=ORIENTED_EDGE('',*,*,#2040,.T.);
#2785=ORIENTED_EDGE('',*,*,#2030,.T.);
#2786=ORIENTED_EDGE('',*,*,#2035,.T.);
#2787=ORIENTED_EDGE('',*,*,#2023,.T.);
#2788=ORIENTED_EDGE('',*,*,#2020,.T.);
#2789=ORIENTED_EDGE('',*,*,#2017,.T.);
#2790=ORIENTED_EDGE('',*,*,#2014,.T.);
#2791=ORIENTED_EDGE('',*,*,#2011,.T.);
#2792=ORIENTED_EDGE('',*,*,#2050,.F.);
#2793=ORIENTED_EDGE('',*,*,#2051,.T.);
#2794=ORIENTED_EDGE('',*,*,#2052,.T.);
#2795=ORIENTED_EDGE('',*,*,#2051,.F.);
#2796=ORIENTED_EDGE('',*,*,#2053,.F.);
#2797=ORIENTED_EDGE('',*,*,#2054,.T.);
#2798=ORIENTED_EDGE('',*,*,#2055,.T.);
#2799=ORIENTED_EDGE('',*,*,#2054,.F.);
#2800=ORIENTED_EDGE('',*,*,#2053,.T.);
#2801=ORIENTED_EDGE('',*,*,#2050,.T.);
#2802=ORIENTED_EDGE('',*,*,#2055,.F.);
#2803=ORIENTED_EDGE('',*,*,#2052,.F.);
#2804=ORIENTED_EDGE('',*,*,#2056,.F.);
#2805=ORIENTED_EDGE('',*,*,#2057,.F.);
#2806=ORIENTED_EDGE('',*,*,#2058,.T.);
#2807=ORIENTED_EDGE('',*,*,#2059,.F.);
#2808=ORIENTED_EDGE('',*,*,#2058,.F.);
#2809=ORIENTED_EDGE('',*,*,#2060,.F.);
#2810=ORIENTED_EDGE('',*,*,#2061,.F.);
#2811=ORIENTED_EDGE('',*,*,#2062,.F.);
#2812=ORIENTED_EDGE('',*,*,#2063,.F.);
#2813=ORIENTED_EDGE('',*,*,#2064,.F.);
#2814=ORIENTED_EDGE('',*,*,#2065,.T.);
#2815=ORIENTED_EDGE('',*,*,#2066,.F.);
#2816=ORIENTED_EDGE('',*,*,#2067,.F.);
#2817=ORIENTED_EDGE('',*,*,#2068,.F.);
#2818=ORIENTED_EDGE('',*,*,#2069,.F.);
#2819=ORIENTED_EDGE('',*,*,#2070,.F.);
#2820=ORIENTED_EDGE('',*,*,#2071,.F.);
#2821=ORIENTED_EDGE('',*,*,#2065,.F.);
#2822=ORIENTED_EDGE('',*,*,#2061,.T.);
#2823=ORIENTED_EDGE('',*,*,#2072,.T.);
#2824=ORIENTED_EDGE('',*,*,#2070,.T.);
#2825=ORIENTED_EDGE('',*,*,#2073,.F.);
#2826=ORIENTED_EDGE('',*,*,#2060,.T.);
#2827=ORIENTED_EDGE('',*,*,#2074,.T.);
#2828=ORIENTED_EDGE('',*,*,#2071,.T.);
#2829=ORIENTED_EDGE('',*,*,#2072,.F.);
#2830=ORIENTED_EDGE('',*,*,#2057,.T.);
#2831=ORIENTED_EDGE('',*,*,#2075,.T.);
#2832=ORIENTED_EDGE('',*,*,#2066,.T.);
#2833=ORIENTED_EDGE('',*,*,#2074,.F.);
#2834=ORIENTED_EDGE('',*,*,#2076,.F.);
#2835=ORIENTED_EDGE('',*,*,#2077,.T.);
#2836=ORIENTED_EDGE('',*,*,#2078,.T.);
#2837=ORIENTED_EDGE('',*,*,#2077,.F.);
#2838=ORIENTED_EDGE('',*,*,#2056,.T.);
#2839=ORIENTED_EDGE('',*,*,#2079,.T.);
#2840=ORIENTED_EDGE('',*,*,#2067,.T.);
#2841=ORIENTED_EDGE('',*,*,#2075,.F.);
#2842=ORIENTED_EDGE('',*,*,#2062,.T.);
#2843=ORIENTED_EDGE('',*,*,#2073,.T.);
#2844=ORIENTED_EDGE('',*,*,#2069,.T.);
#2845=ORIENTED_EDGE('',*,*,#2080,.F.);
#2846=ORIENTED_EDGE('',*,*,#2063,.T.);
#2847=ORIENTED_EDGE('',*,*,#2080,.T.);
#2848=ORIENTED_EDGE('',*,*,#2068,.T.);
#2849=ORIENTED_EDGE('',*,*,#2079,.F.);
#2850=ORIENTED_EDGE('',*,*,#2064,.T.);
#2851=ORIENTED_EDGE('',*,*,#2076,.T.);
#2852=ORIENTED_EDGE('',*,*,#2059,.T.);
#2853=ORIENTED_EDGE('',*,*,#2078,.F.);
#2854=ORIENTED_EDGE('',*,*,#2081,.F.);
#2855=ORIENTED_EDGE('',*,*,#2082,.F.);
#2856=ORIENTED_EDGE('',*,*,#2083,.F.);
#2857=ORIENTED_EDGE('',*,*,#2084,.F.);
#2858=ORIENTED_EDGE('',*,*,#2085,.F.);
#2859=ORIENTED_EDGE('',*,*,#2086,.F.);
#2860=ORIENTED_EDGE('',*,*,#2087,.F.);
#2861=ORIENTED_EDGE('',*,*,#2088,.F.);
#2862=ORIENTED_EDGE('',*,*,#2089,.F.);
#2863=ORIENTED_EDGE('',*,*,#2090,.F.);
#2864=ORIENTED_EDGE('',*,*,#2091,.F.);
#2865=ORIENTED_EDGE('',*,*,#2092,.F.);
#2866=ORIENTED_EDGE('',*,*,#2093,.F.);
#2867=ORIENTED_EDGE('',*,*,#2094,.F.);
#2868=ORIENTED_EDGE('',*,*,#2095,.F.);
#2869=ORIENTED_EDGE('',*,*,#2096,.F.);
#2870=ORIENTED_EDGE('',*,*,#2097,.F.);
#2871=ORIENTED_EDGE('',*,*,#2098,.F.);
#2872=ORIENTED_EDGE('',*,*,#2099,.F.);
#2873=ORIENTED_EDGE('',*,*,#2100,.F.);
#2874=ORIENTED_EDGE('',*,*,#2101,.F.);
#2875=ORIENTED_EDGE('',*,*,#2102,.F.);
#2876=ORIENTED_EDGE('',*,*,#2103,.F.);
#2877=ORIENTED_EDGE('',*,*,#2104,.F.);
#2878=ORIENTED_EDGE('',*,*,#2082,.T.);
#2879=ORIENTED_EDGE('',*,*,#2105,.T.);
#2880=ORIENTED_EDGE('',*,*,#2102,.T.);
#2881=ORIENTED_EDGE('',*,*,#2106,.T.);
#2882=ORIENTED_EDGE('',*,*,#2088,.T.);
#2883=ORIENTED_EDGE('',*,*,#2107,.T.);
#2884=ORIENTED_EDGE('',*,*,#2090,.T.);
#2885=ORIENTED_EDGE('',*,*,#2108,.T.);
#2886=ORIENTED_EDGE('',*,*,#2094,.T.);
#2887=ORIENTED_EDGE('',*,*,#2109,.T.);
#2888=ORIENTED_EDGE('',*,*,#2098,.T.);
#2889=ORIENTED_EDGE('',*,*,#2110,.T.);
#2890=ORIENTED_EDGE('',*,*,#2111,.T.);
#2891=ORIENTED_EDGE('',*,*,#2093,.T.);
#2892=ORIENTED_EDGE('',*,*,#2112,.T.);
#2893=ORIENTED_EDGE('',*,*,#2099,.T.);
#2894=ORIENTED_EDGE('',*,*,#2109,.F.);
#2895=ORIENTED_EDGE('',*,*,#2089,.T.);
#2896=ORIENTED_EDGE('',*,*,#2113,.T.);
#2897=ORIENTED_EDGE('',*,*,#2095,.T.);
#2898=ORIENTED_EDGE('',*,*,#2108,.F.);
#2899=ORIENTED_EDGE('',*,*,#2085,.T.);
#2900=ORIENTED_EDGE('',*,*,#2106,.F.);
#2901=ORIENTED_EDGE('',*,*,#2101,.T.);
#2902=ORIENTED_EDGE('',*,*,#2114,.T.);
#2903=ORIENTED_EDGE('',*,*,#2087,.T.);
#2904=ORIENTED_EDGE('',*,*,#2115,.T.);
#2905=ORIENTED_EDGE('',*,*,#2091,.T.);
#2906=ORIENTED_EDGE('',*,*,#2107,.F.);
#2907=ORIENTED_EDGE('',*,*,#2081,.T.);
#2908=ORIENTED_EDGE('',*,*,#2116,.T.);
#2909=ORIENTED_EDGE('',*,*,#2103,.T.);
#2910=ORIENTED_EDGE('',*,*,#2105,.F.);
#2911=ORIENTED_EDGE('',*,*,#2083,.T.);
#2912=ORIENTED_EDGE('',*,*,#2110,.F.);
#2913=ORIENTED_EDGE('',*,*,#2097,.T.);
#2914=ORIENTED_EDGE('',*,*,#2117,.T.);
#2915=ORIENTED_EDGE('',*,*,#2118,.F.);
#2916=ORIENTED_EDGE('',*,*,#2119,.T.);
#2917=ORIENTED_EDGE('',*,*,#2120,.T.);
#2918=ORIENTED_EDGE('',*,*,#2121,.F.);
#2919=ORIENTED_EDGE('',*,*,#2122,.F.);
#2920=ORIENTED_EDGE('',*,*,#2121,.T.);
#2921=ORIENTED_EDGE('',*,*,#2123,.T.);
#2922=ORIENTED_EDGE('',*,*,#2124,.F.);
#2923=ORIENTED_EDGE('',*,*,#2125,.F.);
#2924=ORIENTED_EDGE('',*,*,#2124,.T.);
#2925=ORIENTED_EDGE('',*,*,#2126,.T.);
#2926=ORIENTED_EDGE('',*,*,#2127,.F.);
#2927=ORIENTED_EDGE('',*,*,#2128,.F.);
#2928=ORIENTED_EDGE('',*,*,#2127,.T.);
#2929=ORIENTED_EDGE('',*,*,#2129,.T.);
#2930=ORIENTED_EDGE('',*,*,#2130,.F.);
#2931=ORIENTED_EDGE('',*,*,#2131,.F.);
#2932=ORIENTED_EDGE('',*,*,#2132,.T.);
#2933=ORIENTED_EDGE('',*,*,#2133,.T.);
#2934=ORIENTED_EDGE('',*,*,#2119,.F.);
#2935=ORIENTED_EDGE('',*,*,#2134,.F.);
#2936=ORIENTED_EDGE('',*,*,#2130,.T.);
#2937=ORIENTED_EDGE('',*,*,#2135,.T.);
#2938=ORIENTED_EDGE('',*,*,#2132,.F.);
#2939=ORIENTED_EDGE('',*,*,#2135,.F.);
#2940=ORIENTED_EDGE('',*,*,#2129,.F.);
#2941=ORIENTED_EDGE('',*,*,#2126,.F.);
#2942=ORIENTED_EDGE('',*,*,#2123,.F.);
#2943=ORIENTED_EDGE('',*,*,#2120,.F.);
#2944=ORIENTED_EDGE('',*,*,#2133,.F.);
#2945=ORIENTED_EDGE('',*,*,#2136,.F.);
#2946=ORIENTED_EDGE('',*,*,#2111,.F.);
#2947=ORIENTED_EDGE('',*,*,#2137,.T.);
#2948=ORIENTED_EDGE('',*,*,#2136,.T.);
#2949=ORIENTED_EDGE('',*,*,#2137,.F.);
#2950=ORIENTED_EDGE('',*,*,#2084,.T.);
#2951=ORIENTED_EDGE('',*,*,#2117,.F.);
#2952=ORIENTED_EDGE('',*,*,#2100,.T.);
#2953=ORIENTED_EDGE('',*,*,#2112,.F.);
#2954=ORIENTED_EDGE('',*,*,#2096,.T.);
#2955=ORIENTED_EDGE('',*,*,#2113,.F.);
#2956=ORIENTED_EDGE('',*,*,#2092,.T.);
#2957=ORIENTED_EDGE('',*,*,#2115,.F.);
#2958=ORIENTED_EDGE('',*,*,#2086,.T.);
#2959=ORIENTED_EDGE('',*,*,#2114,.F.);
#2960=ORIENTED_EDGE('',*,*,#2104,.T.);
#2961=ORIENTED_EDGE('',*,*,#2116,.F.);
#2962=ORIENTED_EDGE('',*,*,#2128,.T.);
#2963=ORIENTED_EDGE('',*,*,#2134,.T.);
#2964=ORIENTED_EDGE('',*,*,#2131,.T.);
#2965=ORIENTED_EDGE('',*,*,#2118,.T.);
#2966=ORIENTED_EDGE('',*,*,#2122,.T.);
#2967=ORIENTED_EDGE('',*,*,#2125,.T.);
#2968=CYLINDRICAL_SURFACE('',#3308,0.275);
#2969=CYLINDRICAL_SURFACE('',#3311,0.275);
#2970=CYLINDRICAL_SURFACE('',#3314,0.425);
#2971=CYLINDRICAL_SURFACE('',#3364,0.21);
#2972=CYLINDRICAL_SURFACE('',#3389,0.2117);
#2973=CYLINDRICAL_SURFACE('',#3402,0.265);
#2974=CYLINDRICAL_SURFACE('',#3406,0.5);
#2975=CYLINDRICAL_SURFACE('',#3424,0.425);
#2976=CYLINDRICAL_SURFACE('',#3432,0.24505);
#2977=CYLINDRICAL_SURFACE('',#3436,0.425);
#2978=CYLINDRICAL_SURFACE('',#3439,0.425000000000001);
#2979=CYLINDRICAL_SURFACE('',#3442,1.5);
#2980=CYLINDRICAL_SURFACE('',#3449,1.5);
#2981=CYLINDRICAL_SURFACE('',#3453,0.3933);
#2982=CYLINDRICAL_SURFACE('',#3480,0.329999999999998);
#2983=CYLINDRICAL_SURFACE('',#3483,0.329999999999998);
#2984=CYLINDRICAL_SURFACE('',#3486,0.329999999999998);
#2985=CYLINDRICAL_SURFACE('',#3489,0.329999999999998);
#2986=CYLINDRICAL_SURFACE('',#3492,0.425000000000001);
#2987=CYLINDRICAL_SURFACE('',#3504,1.5);
#2988=CYLINDRICAL_SURFACE('',#3508,0.42);
#2989=CYLINDRICAL_SURFACE('',#3511,0.8);
#2990=CYLINDRICAL_SURFACE('',#3524,0.338975);
#2991=CYLINDRICAL_SURFACE('',#3533,0.4);
#2992=CYLINDRICAL_SURFACE('',#3536,0.4);
#2993=CYLINDRICAL_SURFACE('',#3539,0.4);
#2994=CYLINDRICAL_SURFACE('',#3542,0.4);
#2995=CYLINDRICAL_SURFACE('',#3545,0.4);
#2996=CYLINDRICAL_SURFACE('',#3548,0.4);
#2997=CYLINDRICAL_SURFACE('',#3559,1.8);
#2998=CYLINDRICAL_SURFACE('',#3561,1.8);
#2999=CYLINDRICAL_SURFACE('',#3563,1.8);
#3000=CYLINDRICAL_SURFACE('',#3565,1.8);
#3001=CYLINDRICAL_SURFACE('',#3567,1.8);
#3002=CYLINDRICAL_SURFACE('',#3569,1.8);
#3003=CYLINDRICAL_SURFACE('',#3579,0.425);
#3004=ADVANCED_FACE('',(#373),#2968,.F.);
#3005=ADVANCED_FACE('',(#374),#2969,.F.);
#3006=ADVANCED_FACE('',(#375),#2970,.F.);
#3007=ADVANCED_FACE('',(#376),#250,.T.);
#3008=ADVANCED_FACE('',(#377),#251,.T.);
#3009=ADVANCED_FACE('',(#378),#252,.T.);
#3010=ADVANCED_FACE('',(#379,#216),#253,.F.);
#3011=ADVANCED_FACE('',(#380,#217,#218),#254,.T.);
#3012=ADVANCED_FACE('',(#381,#219),#255,.T.);
#3013=ADVANCED_FACE('',(#382),#256,.T.);
#3014=ADVANCED_FACE('',(#383),#257,.T.);
#3015=ADVANCED_FACE('',(#384),#258,.T.);
#3016=ADVANCED_FACE('',(#385,#220,#221),#259,.F.);
#3017=ADVANCED_FACE('',(#386),#260,.F.);
#3018=ADVANCED_FACE('',(#387),#261,.F.);
#3019=ADVANCED_FACE('',(#388),#262,.F.);
#3020=ADVANCED_FACE('',(#389),#263,.F.);
#3021=ADVANCED_FACE('',(#390),#264,.F.);
#3022=ADVANCED_FACE('',(#391),#265,.F.);
#3023=ADVANCED_FACE('',(#392),#266,.F.);
#3024=ADVANCED_FACE('',(#393),#267,.F.);
#3025=ADVANCED_FACE('',(#394),#268,.F.);
#3026=ADVANCED_FACE('',(#395),#269,.F.);
#3027=ADVANCED_FACE('',(#396),#270,.F.);
#3028=ADVANCED_FACE('',(#397),#271,.F.);
#3029=ADVANCED_FACE('',(#398),#272,.F.);
#3030=ADVANCED_FACE('',(#399),#273,.F.);
#3031=ADVANCED_FACE('',(#400),#274,.F.);
#3032=ADVANCED_FACE('',(#401),#275,.F.);
#3033=ADVANCED_FACE('',(#402),#276,.F.);
#3034=ADVANCED_FACE('',(#403),#277,.F.);
#3035=ADVANCED_FACE('',(#404),#278,.F.);
#3036=ADVANCED_FACE('',(#405),#279,.F.);
#3037=ADVANCED_FACE('',(#406),#280,.F.);
#3038=ADVANCED_FACE('',(#407),#281,.F.);
#3039=ADVANCED_FACE('',(#408),#282,.F.);
#3040=ADVANCED_FACE('',(#409),#283,.F.);
#3041=ADVANCED_FACE('',(#410),#284,.F.);
#3042=ADVANCED_FACE('',(#411),#285,.F.);
#3043=ADVANCED_FACE('',(#412),#286,.F.);
#3044=ADVANCED_FACE('',(#413),#287,.F.);
#3045=ADVANCED_FACE('',(#414),#288,.F.);
#3046=ADVANCED_FACE('',(#415),#289,.F.);
#3047=ADVANCED_FACE('',(#416),#290,.F.);
#3048=ADVANCED_FACE('',(#417),#291,.F.);
#3049=ADVANCED_FACE('',(#418),#292,.F.);
#3050=ADVANCED_FACE('',(#419),#293,.F.);
#3051=ADVANCED_FACE('',(#420),#294,.F.);
#3052=ADVANCED_FACE('',(#421),#295,.F.);
#3053=ADVANCED_FACE('',(#422),#2971,.F.);
#3054=ADVANCED_FACE('',(#423),#296,.T.);
#3055=ADVANCED_FACE('',(#424),#297,.T.);
#3056=ADVANCED_FACE('',(#425),#298,.T.);
#3057=ADVANCED_FACE('',(#426),#299,.T.);
#3058=ADVANCED_FACE('',(#427),#300,.T.);
#3059=ADVANCED_FACE('',(#428),#301,.T.);
#3060=ADVANCED_FACE('',(#429),#302,.T.);
#3061=ADVANCED_FACE('',(#430),#303,.T.);
#3062=ADVANCED_FACE('',(#431,#222),#304,.T.);
#3063=ADVANCED_FACE('',(#432,#223),#305,.F.);
#3064=ADVANCED_FACE('',(#433),#306,.F.);
#3065=ADVANCED_FACE('',(#434),#307,.T.);
#3066=ADVANCED_FACE('',(#435,#224),#308,.T.);
#3067=ADVANCED_FACE('',(#436),#309,.T.);
#3068=ADVANCED_FACE('',(#437),#310,.T.);
#3069=ADVANCED_FACE('',(#438),#311,.F.);
#3070=ADVANCED_FACE('',(#439),#312,.T.);
#3071=ADVANCED_FACE('',(#440),#313,.T.);
#3072=ADVANCED_FACE('',(#441),#314,.T.);
#3073=ADVANCED_FACE('',(#442),#2972,.F.);
#3074=ADVANCED_FACE('',(#443),#315,.F.);
#3075=ADVANCED_FACE('',(#444),#316,.F.);
#3076=ADVANCED_FACE('',(#445),#317,.T.);
#3077=ADVANCED_FACE('',(#446),#318,.T.);
#3078=ADVANCED_FACE('',(#447),#163,.F.);
#3079=ADVANCED_FACE('',(#448),#2973,.F.);
#3080=ADVANCED_FACE('',(#449,#225),#319,.T.);
#3081=ADVANCED_FACE('',(#450),#2974,.T.);
#3082=ADVANCED_FACE('',(#451,#226),#320,.F.);
#3083=ADVANCED_FACE('',(#452),#321,.F.);
#3084=ADVANCED_FACE('',(#453),#322,.F.);
#3085=ADVANCED_FACE('',(#454),#323,.F.);
#3086=ADVANCED_FACE('',(#455),#324,.F.);
#3087=ADVANCED_FACE('',(#456),#325,.F.);
#3088=ADVANCED_FACE('',(#457),#326,.F.);
#3089=ADVANCED_FACE('',(#458),#327,.F.);
#3090=ADVANCED_FACE('',(#459),#328,.F.);
#3091=ADVANCED_FACE('',(#460),#329,.F.);
#3092=ADVANCED_FACE('',(#461),#330,.T.);
#3093=ADVANCED_FACE('',(#462),#164,.T.);
#3094=ADVANCED_FACE('',(#463),#2975,.T.);
#3095=ADVANCED_FACE('',(#464),#165,.T.);
#3096=ADVANCED_FACE('',(#465,#227),#331,.T.);
#3097=ADVANCED_FACE('',(#466),#166,.T.);
#3098=ADVANCED_FACE('',(#467),#2976,.T.);
#3099=ADVANCED_FACE('',(#468),#2977,.F.);
#3100=ADVANCED_FACE('',(#469),#2978,.F.);
#3101=ADVANCED_FACE('',(#470),#2979,.T.);
#3102=ADVANCED_FACE('',(#471),#332,.T.);
#3103=ADVANCED_FACE('',(#472,#228,#229),#333,.F.);
#3104=ADVANCED_FACE('',(#473),#334,.T.);
#3105=ADVANCED_FACE('',(#474),#2980,.T.);
#3106=ADVANCED_FACE('',(#475,#230,#231),#335,.T.);
#3107=ADVANCED_FACE('',(#476),#2981,.T.);
#3108=ADVANCED_FACE('',(#477),#167,.T.);
#3109=ADVANCED_FACE('',(#478),#336,.T.);
#3110=ADVANCED_FACE('',(#479),#168,.T.);
#3111=ADVANCED_FACE('',(#480),#337,.T.);
#3112=ADVANCED_FACE('',(#481),#338,.T.);
#3113=ADVANCED_FACE('',(#482),#339,.T.);
#3114=ADVANCED_FACE('',(#483),#340,.T.);
#3115=ADVANCED_FACE('',(#484),#341,.T.);
#3116=ADVANCED_FACE('',(#485),#342,.T.);
#3117=ADVANCED_FACE('',(#486),#343,.T.);
#3118=ADVANCED_FACE('',(#487,#232),#344,.F.);
#3119=ADVANCED_FACE('',(#488),#2982,.F.);
#3120=ADVANCED_FACE('',(#489),#2983,.F.);
#3121=ADVANCED_FACE('',(#490),#2984,.F.);
#3122=ADVANCED_FACE('',(#491),#2985,.F.);
#3123=ADVANCED_FACE('',(#492),#2986,.F.);
#3124=ADVANCED_FACE('',(#493),#345,.T.);
#3125=ADVANCED_FACE('',(#494),#346,.T.);
#3126=ADVANCED_FACE('',(#495),#347,.T.);
#3127=ADVANCED_FACE('',(#496),#348,.T.);
#3128=ADVANCED_FACE('',(#497),#349,.T.);
#3129=ADVANCED_FACE('',(#498),#350,.T.);
#3130=ADVANCED_FACE('',(#499,#233,#234,#235,#236,#237),#351,.T.);
#3131=ADVANCED_FACE('',(#500),#352,.T.);
#3132=ADVANCED_FACE('',(#501),#2987,.T.);
#3133=ADVANCED_FACE('',(#502,#238,#239,#240,#241,#242),#353,.F.);
#3134=ADVANCED_FACE('',(#503),#2988,.F.);
#3135=ADVANCED_FACE('',(#504),#2989,.T.);
#3136=ADVANCED_FACE('',(#505,#243),#354,.T.);
#3137=ADVANCED_FACE('',(#506,#244),#355,.F.);
#3138=ADVANCED_FACE('',(#507),#169,.T.);
#3139=ADVANCED_FACE('',(#508),#170,.T.);
#3140=ADVANCED_FACE('',(#509),#356,.T.);
#3141=ADVANCED_FACE('',(#510),#357,.T.);
#3142=ADVANCED_FACE('',(#511),#358,.T.);
#3143=ADVANCED_FACE('',(#512),#2990,.F.);
#3144=ADVANCED_FACE('',(#513),#359,.T.);
#3145=ADVANCED_FACE('',(#514),#360,.T.);
#3146=ADVANCED_FACE('',(#515),#361,.T.);
#3147=ADVANCED_FACE('',(#516,#245),#362,.T.);
#3148=ADVANCED_FACE('',(#517,#246),#363,.F.);
#3149=ADVANCED_FACE('',(#518),#2991,.F.);
#3150=ADVANCED_FACE('',(#519),#2992,.F.);
#3151=ADVANCED_FACE('',(#520),#2993,.F.);
#3152=ADVANCED_FACE('',(#521),#2994,.F.);
#3153=ADVANCED_FACE('',(#522),#2995,.F.);
#3154=ADVANCED_FACE('',(#523),#2996,.F.);
#3155=ADVANCED_FACE('',(#524,#247),#364,.T.);
#3156=ADVANCED_FACE('',(#525),#2997,.T.);
#3157=ADVANCED_FACE('',(#526),#2998,.T.);
#3158=ADVANCED_FACE('',(#527),#2999,.T.);
#3159=ADVANCED_FACE('',(#528),#3000,.T.);
#3160=ADVANCED_FACE('',(#529),#3001,.T.);
#3161=ADVANCED_FACE('',(#530),#3002,.T.);
#3162=ADVANCED_FACE('',(#531),#365,.F.);
#3163=ADVANCED_FACE('',(#532),#366,.F.);
#3164=ADVANCED_FACE('',(#533),#367,.F.);
#3165=ADVANCED_FACE('',(#534),#368,.F.);
#3166=ADVANCED_FACE('',(#535),#369,.F.);
#3167=ADVANCED_FACE('',(#536),#370,.F.);
#3168=ADVANCED_FACE('',(#537,#248),#371,.F.);
#3169=ADVANCED_FACE('',(#538),#3003,.F.);
#3170=ADVANCED_FACE('',(#539,#249),#372,.F.);
#3171=CLOSED_SHELL('',(#3004,#3005,#3006,#3007,#3008,#3009,#3010,#3011,
#3012,#3013,#3014,#3015,#3016));
#3172=CLOSED_SHELL('',(#3017,#3018,#3019,#3020,#3021,#3022,#3023,#3024,
#3025,#3026,#3027,#3028,#3029,#3030,#3031,#3032,#3033,#3034,#3035,#3036,
#3037,#3038,#3039,#3040,#3041,#3042,#3043,#3044,#3045,#3046,#3047,#3048,
#3049,#3050,#3051,#3052,#3053,#3054,#3055,#3056,#3057,#3058,#3059,#3060,
#3061,#3062,#3063));
#3173=CLOSED_SHELL('',(#3064,#3065,#3066,#3067,#3068,#3069,#3070,#3071,
#3072,#3073,#3074,#3075,#3076,#3077));
#3174=CLOSED_SHELL('',(#3078,#3079,#3080,#3081,#3082));
#3175=CLOSED_SHELL('',(#3083,#3084,#3085,#3086,#3087,#3088,#3089,#3090));
#3176=CLOSED_SHELL('',(#3091,#3092,#3093,#3094,#3095,#3096,#3097,#3098));
#3177=CLOSED_SHELL('',(#3099,#3100,#3101,#3102,#3103,#3104,#3105,#3106));
#3178=CLOSED_SHELL('',(#3107,#3108,#3109,#3110,#3111,#3112,#3113,#3114,
#3115,#3116,#3117,#3118));
#3179=CLOSED_SHELL('',(#3119,#3120,#3121,#3122,#3123,#3124,#3125,#3126,
#3127,#3128,#3129,#3130,#3131,#3132,#3133));
#3180=CLOSED_SHELL('',(#3134,#3135,#3136,#3137));
#3181=CLOSED_SHELL('',(#3138,#3139,#3140,#3141,#3142,#3143,#3144,#3145,
#3146,#3147,#3148));
#3182=CLOSED_SHELL('',(#3149,#3150,#3151,#3152,#3153,#3154,#3155,#3156,
#3157,#3158,#3159,#3160,#3161,#3162,#3163,#3164,#3165,#3166,#3167,#3168,
#3169,#3170));
#3183=DERIVED_UNIT_ELEMENT(#3205,1.);
#3184=DERIVED_UNIT_ELEMENT(#5494,-3.);
#3185=DERIVED_UNIT_ELEMENT(#3205,1.);
#3186=DERIVED_UNIT_ELEMENT(#5494,-3.);
#3187=DERIVED_UNIT_ELEMENT(#3205,1.);
#3188=DERIVED_UNIT_ELEMENT(#5494,-3.);
#3189=DERIVED_UNIT_ELEMENT(#3205,1.);
#3190=DERIVED_UNIT_ELEMENT(#5494,-3.);
#3191=DERIVED_UNIT_ELEMENT(#3205,1.);
#3192=DERIVED_UNIT_ELEMENT(#5494,-3.);
#3193=DERIVED_UNIT_ELEMENT(#3205,1.);
#3194=DERIVED_UNIT_ELEMENT(#5494,-3.);
#3195=DERIVED_UNIT_ELEMENT(#3205,1.);
#3196=DERIVED_UNIT_ELEMENT(#5494,-3.);
#3197=DERIVED_UNIT_ELEMENT(#3205,1.);
#3198=DERIVED_UNIT_ELEMENT(#5494,-3.);
#3199=DERIVED_UNIT_ELEMENT(#3205,1.);
#3200=DERIVED_UNIT_ELEMENT(#5494,-3.);
#3201=DERIVED_UNIT_ELEMENT(#3205,1.);
#3202=DERIVED_UNIT_ELEMENT(#5494,-3.);
#3203=DERIVED_UNIT_ELEMENT(#3205,1.);
#3204=DERIVED_UNIT_ELEMENT(#5494,-3.);
#3205=(
MASS_UNIT()
NAMED_UNIT(*)
SI_UNIT(.KILO.,.GRAM.)
);
#3206=DERIVED_UNIT((#3183,#3184));
#3207=DERIVED_UNIT((#3185,#3186));
#3208=DERIVED_UNIT((#3187,#3188));
#3209=DERIVED_UNIT((#3189,#3190));
#3210=DERIVED_UNIT((#3191,#3192));
#3211=DERIVED_UNIT((#3193,#3194));
#3212=DERIVED_UNIT((#3195,#3196));
#3213=DERIVED_UNIT((#3197,#3198));
#3214=DERIVED_UNIT((#3199,#3200));
#3215=DERIVED_UNIT((#3201,#3202));
#3216=DERIVED_UNIT((#3203,#3204));
#3217=MEASURE_REPRESENTATION_ITEM('density measure',
POSITIVE_RATIO_MEASURE(7850.),#3206);
#3218=MEASURE_REPRESENTATION_ITEM('density measure',
POSITIVE_RATIO_MEASURE(7850.),#3207);
#3219=MEASURE_REPRESENTATION_ITEM('density measure',
POSITIVE_RATIO_MEASURE(7850.),#3208);
#3220=MEASURE_REPRESENTATION_ITEM('density measure',
POSITIVE_RATIO_MEASURE(7850.),#3209);
#3221=MEASURE_REPRESENTATION_ITEM('density measure',
POSITIVE_RATIO_MEASURE(7850.),#3210);
#3222=MEASURE_REPRESENTATION_ITEM('density measure',
POSITIVE_RATIO_MEASURE(7850.),#3211);
#3223=MEASURE_REPRESENTATION_ITEM('density measure',
POSITIVE_RATIO_MEASURE(7850.),#3212);
#3224=MEASURE_REPRESENTATION_ITEM('density measure',
POSITIVE_RATIO_MEASURE(7850.),#3213);
#3225=MEASURE_REPRESENTATION_ITEM('density measure',
POSITIVE_RATIO_MEASURE(7850.),#3214);
#3226=MEASURE_REPRESENTATION_ITEM('density measure',
POSITIVE_RATIO_MEASURE(7850.),#3215);
#3227=MEASURE_REPRESENTATION_ITEM('density measure',
POSITIVE_RATIO_MEASURE(7850.),#3216);
#3228=PROPERTY_DEFINITION_REPRESENTATION(#3283,#3250);
#3229=PROPERTY_DEFINITION_REPRESENTATION(#3284,#3251);
#3230=PROPERTY_DEFINITION_REPRESENTATION(#3285,#3252);
#3231=PROPERTY_DEFINITION_REPRESENTATION(#3286,#3253);
#3232=PROPERTY_DEFINITION_REPRESENTATION(#3287,#3254);
#3233=PROPERTY_DEFINITION_REPRESENTATION(#3288,#3255);
#3234=PROPERTY_DEFINITION_REPRESENTATION(#3289,#3256);
#3235=PROPERTY_DEFINITION_REPRESENTATION(#3290,#3257);
#3236=PROPERTY_DEFINITION_REPRESENTATION(#3291,#3258);
#3237=PROPERTY_DEFINITION_REPRESENTATION(#3292,#3259);
#3238=PROPERTY_DEFINITION_REPRESENTATION(#3293,#3260);
#3239=PROPERTY_DEFINITION_REPRESENTATION(#3294,#3261);
#3240=PROPERTY_DEFINITION_REPRESENTATION(#3295,#3262);
#3241=PROPERTY_DEFINITION_REPRESENTATION(#3296,#3263);
#3242=PROPERTY_DEFINITION_REPRESENTATION(#3297,#3264);
#3243=PROPERTY_DEFINITION_REPRESENTATION(#3298,#3265);
#3244=PROPERTY_DEFINITION_REPRESENTATION(#3299,#3266);
#3245=PROPERTY_DEFINITION_REPRESENTATION(#3300,#3267);
#3246=PROPERTY_DEFINITION_REPRESENTATION(#3301,#3268);
#3247=PROPERTY_DEFINITION_REPRESENTATION(#3302,#3269);
#3248=PROPERTY_DEFINITION_REPRESENTATION(#3303,#3270);
#3249=PROPERTY_DEFINITION_REPRESENTATION(#3304,#3271);
#3250=REPRESENTATION('material name',(#3272),#5478);
#3251=REPRESENTATION('density',(#3217),#5478);
#3252=REPRESENTATION('material name',(#3273),#5479);
#3253=REPRESENTATION('density',(#3218),#5479);
#3254=REPRESENTATION('material name',(#3274),#5480);
#3255=REPRESENTATION('density',(#3219),#5480);
#3256=REPRESENTATION('material name',(#3275),#5481);
#3257=REPRESENTATION('density',(#3220),#5481);
#3258=REPRESENTATION('material name',(#3276),#5482);
#3259=REPRESENTATION('density',(#3221),#5482);
#3260=REPRESENTATION('material name',(#3277),#5485);
#3261=REPRESENTATION('density',(#3222),#5485);
#3262=REPRESENTATION('material name',(#3278),#5486);
#3263=REPRESENTATION('density',(#3223),#5486);
#3264=REPRESENTATION('material name',(#3279),#5488);
#3265=REPRESENTATION('density',(#3224),#5488);
#3266=REPRESENTATION('material name',(#3280),#5489);
#3267=REPRESENTATION('density',(#3225),#5489);
#3268=REPRESENTATION('material name',(#3281),#5490);
#3269=REPRESENTATION('density',(#3226),#5490);
#3270=REPRESENTATION('material name',(#3282),#5491);
#3271=REPRESENTATION('density',(#3227),#5491);
#3272=DESCRIPTIVE_REPRESENTATION_ITEM('Steel','Steel');
#3273=DESCRIPTIVE_REPRESENTATION_ITEM('Steel','Steel');
#3274=DESCRIPTIVE_REPRESENTATION_ITEM('Steel','Steel');
#3275=DESCRIPTIVE_REPRESENTATION_ITEM('Steel','Steel');
#3276=DESCRIPTIVE_REPRESENTATION_ITEM('Steel','Steel');
#3277=DESCRIPTIVE_REPRESENTATION_ITEM('Steel','Steel');
#3278=DESCRIPTIVE_REPRESENTATION_ITEM('Steel','Steel');
#3279=DESCRIPTIVE_REPRESENTATION_ITEM('Steel','Steel');
#3280=DESCRIPTIVE_REPRESENTATION_ITEM('Steel','Steel');
#3281=DESCRIPTIVE_REPRESENTATION_ITEM('Steel','Steel');
#3282=DESCRIPTIVE_REPRESENTATION_ITEM('Steel','Steel');
#3283=PROPERTY_DEFINITION('material property','material name',#5581);
#3284=PROPERTY_DEFINITION('material property','density of part',#5581);
#3285=PROPERTY_DEFINITION('material property','material name',#5582);
#3286=PROPERTY_DEFINITION('material property','density of part',#5582);
#3287=PROPERTY_DEFINITION('material property','material name',#5583);
#3288=PROPERTY_DEFINITION('material property','density of part',#5583);
#3289=PROPERTY_DEFINITION('material property','material name',#5584);
#3290=PROPERTY_DEFINITION('material property','density of part',#5584);
#3291=PROPERTY_DEFINITION('material property','material name',#5585);
#3292=PROPERTY_DEFINITION('material property','density of part',#5585);
#3293=PROPERTY_DEFINITION('material property','material name',#5588);
#3294=PROPERTY_DEFINITION('material property','density of part',#5588);
#3295=PROPERTY_DEFINITION('material property','material name',#5589);
#3296=PROPERTY_DEFINITION('material property','density of part',#5589);
#3297=PROPERTY_DEFINITION('material property','material name',#5591);
#3298=PROPERTY_DEFINITION('material property','density of part',#5591);
#3299=PROPERTY_DEFINITION('material property','material name',#5592);
#3300=PROPERTY_DEFINITION('material property','density of part',#5592);
#3301=PROPERTY_DEFINITION('material property','material name',#5593);
#3302=PROPERTY_DEFINITION('material property','density of part',#5593);
#3303=PROPERTY_DEFINITION('material property','material name',#5594);
#3304=PROPERTY_DEFINITION('material property','density of part',#5594);
#3305=AXIS2_PLACEMENT_3D('',#4518,#3605,#3606);
#3306=AXIS2_PLACEMENT_3D('',#4519,#3607,#3608);
#3307=AXIS2_PLACEMENT_3D('',#4520,#3609,#3610);
#3308=AXIS2_PLACEMENT_3D('',#4521,#3611,#3612);
#3309=AXIS2_PLACEMENT_3D('',#4523,#3613,#3614);
#3310=AXIS2_PLACEMENT_3D('',#4526,#3616,#3617);
#3311=AXIS2_PLACEMENT_3D('',#4527,#3618,#3619);
#3312=AXIS2_PLACEMENT_3D('',#4529,#3620,#3621);
#3313=AXIS2_PLACEMENT_3D('',#4532,#3623,#3624);
#3314=AXIS2_PLACEMENT_3D('',#4533,#3625,#3626);
#3315=AXIS2_PLACEMENT_3D('',#4535,#3627,#3628);
#3316=AXIS2_PLACEMENT_3D('',#4538,#3630,#3631);
#3317=AXIS2_PLACEMENT_3D('',#4539,#3632,#3633);
#3318=AXIS2_PLACEMENT_3D('',#4548,#3638,#3639);
#3319=AXIS2_PLACEMENT_3D('',#4557,#3644,#3645);
#3320=AXIS2_PLACEMENT_3D('',#4560,#3648,#3649);
#3321=AXIS2_PLACEMENT_3D('',#4562,#3651,#3652);
#3322=AXIS2_PLACEMENT_3D('',#4572,#3658,#3659);
#3323=AXIS2_PLACEMENT_3D('',#4578,#3663,#3664);
#3324=AXIS2_PLACEMENT_3D('',#4582,#3667,#3668);
#3325=AXIS2_PLACEMENT_3D('',#4586,#3671,#3672);
#3326=AXIS2_PLACEMENT_3D('',#4588,#3674,#3675);
#3327=AXIS2_PLACEMENT_3D('',#4589,#3676,#3677);
#3328=AXIS2_PLACEMENT_3D('',#4590,#3678,#3679);
#3329=AXIS2_PLACEMENT_3D('',#4599,#3684,#3685);
#3330=AXIS2_PLACEMENT_3D('',#4605,#3689,#3690);
#3331=AXIS2_PLACEMENT_3D('',#4611,#3694,#3695);
#3332=AXIS2_PLACEMENT_3D('',#4617,#3699,#3700);
#3333=AXIS2_PLACEMENT_3D('',#4623,#3704,#3705);
#3334=AXIS2_PLACEMENT_3D('',#4629,#3709,#3710);
#3335=AXIS2_PLACEMENT_3D('',#4635,#3714,#3715);
#3336=AXIS2_PLACEMENT_3D('',#4641,#3719,#3720);
#3337=AXIS2_PLACEMENT_3D('',#4647,#3724,#3725);
#3338=AXIS2_PLACEMENT_3D('',#4656,#3730,#3731);
#3339=AXIS2_PLACEMENT_3D('',#4662,#3735,#3736);
#3340=AXIS2_PLACEMENT_3D('',#4668,#3740,#3741);
#3341=AXIS2_PLACEMENT_3D('',#4674,#3745,#3746);
#3342=AXIS2_PLACEMENT_3D('',#4680,#3750,#3751);
#3343=AXIS2_PLACEMENT_3D('',#4686,#3755,#3756);
#3344=AXIS2_PLACEMENT_3D('',#4692,#3760,#3761);
#3345=AXIS2_PLACEMENT_3D('',#4698,#3765,#3766);
#3346=AXIS2_PLACEMENT_3D('',#4704,#3770,#3771);
#3347=AXIS2_PLACEMENT_3D('',#4713,#3776,#3777);
#3348=AXIS2_PLACEMENT_3D('',#4719,#3781,#3782);
#3349=AXIS2_PLACEMENT_3D('',#4725,#3786,#3787);
#3350=AXIS2_PLACEMENT_3D('',#4731,#3791,#3792);
#3351=AXIS2_PLACEMENT_3D('',#4737,#3796,#3797);
#3352=AXIS2_PLACEMENT_3D('',#4743,#3801,#3802);
#3353=AXIS2_PLACEMENT_3D('',#4749,#3806,#3807);
#3354=AXIS2_PLACEMENT_3D('',#4755,#3811,#3812);
#3355=AXIS2_PLACEMENT_3D('',#4761,#3816,#3817);
#3356=AXIS2_PLACEMENT_3D('',#4770,#3822,#3823);
#3357=AXIS2_PLACEMENT_3D('',#4776,#3827,#3828);
#3358=AXIS2_PLACEMENT_3D('',#4782,#3832,#3833);
#3359=AXIS2_PLACEMENT_3D('',#4788,#3837,#3838);
#3360=AXIS2_PLACEMENT_3D('',#4794,#3842,#3843);
#3361=AXIS2_PLACEMENT_3D('',#4800,#3847,#3848);
#3362=AXIS2_PLACEMENT_3D('',#4806,#3852,#3853);
#3363=AXIS2_PLACEMENT_3D('',#4812,#3857,#3858);
#3364=AXIS2_PLACEMENT_3D('',#4818,#3862,#3863);
#3365=AXIS2_PLACEMENT_3D('',#4820,#3864,#3865);
#3366=AXIS2_PLACEMENT_3D('',#4823,#3867,#3868);
#3367=AXIS2_PLACEMENT_3D('',#4824,#3869,#3870);
#3368=AXIS2_PLACEMENT_3D('',#4830,#3874,#3875);
#3369=AXIS2_PLACEMENT_3D('',#4836,#3879,#3880);
#3370=AXIS2_PLACEMENT_3D('',#4839,#3883,#3884);
#3371=AXIS2_PLACEMENT_3D('',#4845,#3888,#3889);
#3372=AXIS2_PLACEMENT_3D('',#4848,#3892,#3893);
#3373=AXIS2_PLACEMENT_3D('',#4854,#3897,#3898);
#3374=AXIS2_PLACEMENT_3D('',#4857,#3901,#3902);
#3375=AXIS2_PLACEMENT_3D('',#4860,#3905,#3906);
#3376=AXIS2_PLACEMENT_3D('',#4861,#3907,#3908);
#3377=AXIS2_PLACEMENT_3D('',#4862,#3909,#3910);
#3378=AXIS2_PLACEMENT_3D('',#4863,#3911,#3912);
#3379=AXIS2_PLACEMENT_3D('',#4872,#3917,#3918);
#3380=AXIS2_PLACEMENT_3D('',#4878,#3922,#3923);
#3381=AXIS2_PLACEMENT_3D('',#4885,#3927,#3928);
#3382=AXIS2_PLACEMENT_3D('',#4886,#3929,#3930);
#3383=AXIS2_PLACEMENT_3D('',#4900,#3938,#3939);
#3384=AXIS2_PLACEMENT_3D('',#4904,#3942,#3943);
#3385=AXIS2_PLACEMENT_3D('',#4908,#3946,#3947);
#3386=AXIS2_PLACEMENT_3D('',#4918,#3953,#3954);
#3387=AXIS2_PLACEMENT_3D('',#4920,#3956,#3957);
#3388=AXIS2_PLACEMENT_3D('',#4924,#3959,#3960);
#3389=AXIS2_PLACEMENT_3D('',#4926,#3962,#3963);
#3390=AXIS2_PLACEMENT_3D('',#4928,#3964,#3965);
#3391=AXIS2_PLACEMENT_3D('',#4931,#3967,#3968);
#3392=AXIS2_PLACEMENT_3D('',#4933,#3969,#3970);
#3393=AXIS2_PLACEMENT_3D('',#4934,#3971,#3972);
#3394=AXIS2_PLACEMENT_3D('',#4935,#3973,#3974);
#3395=AXIS2_PLACEMENT_3D('',#4937,#3976,#3977);
#3396=AXIS2_PLACEMENT_3D('',#4939,#3979,#3980);
#3397=AXIS2_PLACEMENT_3D('',#4941,#3982,#3983);
#3398=AXIS2_PLACEMENT_3D('',#4942,#3984,#3985);
#3399=AXIS2_PLACEMENT_3D('',#4943,#3986,#3987);
#3400=AXIS2_PLACEMENT_3D('',#4945,#3988,#3989);
#3401=AXIS2_PLACEMENT_3D('',#4948,#3991,#3992);
#3402=AXIS2_PLACEMENT_3D('',#4949,#3993,#3994);
#3403=AXIS2_PLACEMENT_3D('',#4952,#3996,#3997);
#3404=AXIS2_PLACEMENT_3D('',#4953,#3998,#3999);
#3405=AXIS2_PLACEMENT_3D('',#4955,#4000,#4001);
#3406=AXIS2_PLACEMENT_3D('',#4956,#4002,#4003);
#3407=AXIS2_PLACEMENT_3D('',#4959,#4005,#4006);
#3408=AXIS2_PLACEMENT_3D('',#4960,#4007,#4008);
#3409=AXIS2_PLACEMENT_3D('',#4961,#4009,#4010);
#3410=AXIS2_PLACEMENT_3D('',#4962,#4011,#4012);
#3411=AXIS2_PLACEMENT_3D('',#4971,#4017,#4018);
#3412=AXIS2_PLACEMENT_3D('',#4977,#4022,#4023);
#3413=AXIS2_PLACEMENT_3D('',#4983,#4027,#4028);
#3414=AXIS2_PLACEMENT_3D('',#4989,#4032,#4033);
#3415=AXIS2_PLACEMENT_3D('',#4995,#4037,#4038);
#3416=AXIS2_PLACEMENT_3D('',#4998,#4041,#4042);
#3417=AXIS2_PLACEMENT_3D('',#4999,#4043,#4044);
#3418=AXIS2_PLACEMENT_3D('',#5000,#4045,#4046);
#3419=AXIS2_PLACEMENT_3D('',#5002,#4047,#4048);
#3420=AXIS2_PLACEMENT_3D('',#5003,#4049,#4050);
#3421=AXIS2_PLACEMENT_3D('',#5005,#4051,#4052);
#3422=AXIS2_PLACEMENT_3D('',#5006,#4053,#4054);
#3423=AXIS2_PLACEMENT_3D('',#5008,#4055,#4056);
#3424=AXIS2_PLACEMENT_3D('',#5010,#4058,#4059);
#3425=AXIS2_PLACEMENT_3D('',#5012,#4060,#4061);
#3426=AXIS2_PLACEMENT_3D('',#5014,#4063,#4064);
#3427=AXIS2_PLACEMENT_3D('',#5016,#4065,#4066);
#3428=AXIS2_PLACEMENT_3D('',#5018,#4068,#4069);
#3429=AXIS2_PLACEMENT_3D('',#5020,#4070,#4071);
#3430=AXIS2_PLACEMENT_3D('',#5021,#4072,#4073);
#3431=AXIS2_PLACEMENT_3D('',#5023,#4074,#4075);
#3432=AXIS2_PLACEMENT_3D('',#5025,#4077,#4078);
#3433=AXIS2_PLACEMENT_3D('',#5027,#4080,#4081);
#3434=AXIS2_PLACEMENT_3D('',#5028,#4082,#4083);
#3435=AXIS2_PLACEMENT_3D('',#5029,#4084,#4085);
#3436=AXIS2_PLACEMENT_3D('',#5030,#4086,#4087);
#3437=AXIS2_PLACEMENT_3D('',#5032,#4088,#4089);
#3438=AXIS2_PLACEMENT_3D('',#5035,#4091,#4092);
#3439=AXIS2_PLACEMENT_3D('',#5036,#4093,#4094);
#3440=AXIS2_PLACEMENT_3D('',#5038,#4095,#4096);
#3441=AXIS2_PLACEMENT_3D('',#5041,#4098,#4099);
#3442=AXIS2_PLACEMENT_3D('',#5042,#4100,#4101);
#3443=AXIS2_PLACEMENT_3D('',#5047,#4103,#4104);
#3444=AXIS2_PLACEMENT_3D('',#5050,#4106,#4107);
#3445=AXIS2_PLACEMENT_3D('',#5051,#4108,#4109);
#3446=AXIS2_PLACEMENT_3D('',#5057,#4113,#4114);
#3447=AXIS2_PLACEMENT_3D('',#5060,#4116,#4117);
#3448=AXIS2_PLACEMENT_3D('',#5061,#4118,#4119);
#3449=AXIS2_PLACEMENT_3D('',#5065,#4122,#4123);
#3450=AXIS2_PLACEMENT_3D('',#5066,#4124,#4125);
#3451=AXIS2_PLACEMENT_3D('',#5067,#4126,#4127);
#3452=AXIS2_PLACEMENT_3D('',#5068,#4128,#4129);
#3453=AXIS2_PLACEMENT_3D('',#5069,#4130,#4131);
#3454=AXIS2_PLACEMENT_3D('',#5071,#4132,#4133);
#3455=AXIS2_PLACEMENT_3D('',#5074,#4135,#4136);
#3456=AXIS2_PLACEMENT_3D('',#5075,#4137,#4138);
#3457=AXIS2_PLACEMENT_3D('',#5077,#4139,#4140);
#3458=AXIS2_PLACEMENT_3D('',#5079,#4142,#4143);
#3459=AXIS2_PLACEMENT_3D('',#5080,#4144,#4145);
#3460=AXIS2_PLACEMENT_3D('',#5082,#4146,#4147);
#3461=AXIS2_PLACEMENT_3D('',#5108,#4149,#4150);
#3462=AXIS2_PLACEMENT_3D('',#5114,#4154,#4155);
#3463=AXIS2_PLACEMENT_3D('',#5118,#4158,#4159);
#3464=AXIS2_PLACEMENT_3D('',#5122,#4162,#4163);
#3465=AXIS2_PLACEMENT_3D('',#5126,#4166,#4167);
#3466=AXIS2_PLACEMENT_3D('',#5130,#4170,#4171);
#3467=AXIS2_PLACEMENT_3D('',#5132,#4173,#4174);
#3468=AXIS2_PLACEMENT_3D('',#5133,#4175,#4176);
#3469=AXIS2_PLACEMENT_3D('',#5134,#4177,#4178);
#3470=AXIS2_PLACEMENT_3D('',#5135,#4179,#4180);
#3471=AXIS2_PLACEMENT_3D('',#5136,#4181,#4182);
#3472=AXIS2_PLACEMENT_3D('',#5137,#4183,#4184);
#3473=AXIS2_PLACEMENT_3D('',#5138,#4185,#4186);
#3474=AXIS2_PLACEMENT_3D('',#5139,#4187,#4188);
#3475=AXIS2_PLACEMENT_3D('',#5140,#4189,#4190);
#3476=AXIS2_PLACEMENT_3D('',#5141,#4191,#4192);
#3477=AXIS2_PLACEMENT_3D('',#5142,#4193,#4194);
#3478=AXIS2_PLACEMENT_3D('',#5143,#4195,#4196);
#3479=AXIS2_PLACEMENT_3D('',#5144,#4197,#4198);
#3480=AXIS2_PLACEMENT_3D('',#5145,#4199,#4200);
#3481=AXIS2_PLACEMENT_3D('',#5147,#4201,#4202);
#3482=AXIS2_PLACEMENT_3D('',#5150,#4204,#4205);
#3483=AXIS2_PLACEMENT_3D('',#5151,#4206,#4207);
#3484=AXIS2_PLACEMENT_3D('',#5153,#4208,#4209);
#3485=AXIS2_PLACEMENT_3D('',#5156,#4211,#4212);
#3486=AXIS2_PLACEMENT_3D('',#5157,#4213,#4214);
#3487=AXIS2_PLACEMENT_3D('',#5159,#4215,#4216);
#3488=AXIS2_PLACEMENT_3D('',#5162,#4218,#4219);
#3489=AXIS2_PLACEMENT_3D('',#5163,#4220,#4221);
#3490=AXIS2_PLACEMENT_3D('',#5165,#4222,#4223);
#3491=AXIS2_PLACEMENT_3D('',#5168,#4225,#4226);
#3492=AXIS2_PLACEMENT_3D('',#5169,#4227,#4228);
#3493=AXIS2_PLACEMENT_3D('',#5171,#4229,#4230);
#3494=AXIS2_PLACEMENT_3D('',#5174,#4232,#4233);
#3495=AXIS2_PLACEMENT_3D('',#5175,#4234,#4235);
#3496=AXIS2_PLACEMENT_3D('',#5184,#4240,#4241);
#3497=AXIS2_PLACEMENT_3D('',#5193,#4246,#4247);
#3498=AXIS2_PLACEMENT_3D('',#5199,#4251,#4252);
#3499=AXIS2_PLACEMENT_3D('',#5205,#4256,#4257);
#3500=AXIS2_PLACEMENT_3D('',#5208,#4260,#4261);
#3501=AXIS2_PLACEMENT_3D('',#5214,#4265,#4266);
#3502=AXIS2_PLACEMENT_3D('',#5217,#4268,#4269);
#3503=AXIS2_PLACEMENT_3D('',#5218,#4270,#4271);
#3504=AXIS2_PLACEMENT_3D('',#5222,#4274,#4275);
#3505=AXIS2_PLACEMENT_3D('',#5223,#4276,#4277);
#3506=AXIS2_PLACEMENT_3D('',#5224,#4278,#4279);
#3507=AXIS2_PLACEMENT_3D('',#5225,#4280,#4281);
#3508=AXIS2_PLACEMENT_3D('',#5226,#4282,#4283);
#3509=AXIS2_PLACEMENT_3D('',#5228,#4284,#4285);
#3510=AXIS2_PLACEMENT_3D('',#5231,#4287,#4288);
#3511=AXIS2_PLACEMENT_3D('',#5232,#4289,#4290);
#3512=AXIS2_PLACEMENT_3D('',#5234,#4291,#4292);
#3513=AXIS2_PLACEMENT_3D('',#5237,#4294,#4295);
#3514=AXIS2_PLACEMENT_3D('',#5238,#4296,#4297);
#3515=AXIS2_PLACEMENT_3D('',#5239,#4298,#4299);
#3516=AXIS2_PLACEMENT_3D('',#5240,#4300,#4301);
#3517=AXIS2_PLACEMENT_3D('',#5241,#4302,#4303);
#3518=AXIS2_PLACEMENT_3D('',#5253,#4305,#4306);
#3519=AXIS2_PLACEMENT_3D('',#5269,#4307,#4308);
#3520=AXIS2_PLACEMENT_3D('',#5271,#4309,#4310);
#3521=AXIS2_PLACEMENT_3D('',#5297,#4312,#4313);
#3522=AXIS2_PLACEMENT_3D('',#5300,#4316,#4317);
#3523=AXIS2_PLACEMENT_3D('',#5302,#4319,#4320);
#3524=AXIS2_PLACEMENT_3D('',#5304,#4322,#4323);
#3525=AXIS2_PLACEMENT_3D('',#5306,#4324,#4325);
#3526=AXIS2_PLACEMENT_3D('',#5309,#4327,#4328);
#3527=AXIS2_PLACEMENT_3D('',#5310,#4329,#4330);
#3528=AXIS2_PLACEMENT_3D('',#5312,#4332,#4333);
#3529=AXIS2_PLACEMENT_3D('',#5314,#4335,#4336);
#3530=AXIS2_PLACEMENT_3D('',#5315,#4337,#4338);
#3531=AXIS2_PLACEMENT_3D('',#5316,#4339,#4340);
#3532=AXIS2_PLACEMENT_3D('',#5317,#4341,#4342);
#3533=AXIS2_PLACEMENT_3D('',#5318,#4343,#4344);
#3534=AXIS2_PLACEMENT_3D('',#5323,#4346,#4347);
#3535=AXIS2_PLACEMENT_3D('',#5326,#4349,#4350);
#3536=AXIS2_PLACEMENT_3D('',#5327,#4351,#4352);
#3537=AXIS2_PLACEMENT_3D('',#5332,#4354,#4355);
#3538=AXIS2_PLACEMENT_3D('',#5335,#4357,#4358);
#3539=AXIS2_PLACEMENT_3D('',#5336,#4359,#4360);
#3540=AXIS2_PLACEMENT_3D('',#5341,#4362,#4363);
#3541=AXIS2_PLACEMENT_3D('',#5344,#4365,#4366);
#3542=AXIS2_PLACEMENT_3D('',#5345,#4367,#4368);
#3543=AXIS2_PLACEMENT_3D('',#5350,#4370,#4371);
#3544=AXIS2_PLACEMENT_3D('',#5353,#4373,#4374);
#3545=AXIS2_PLACEMENT_3D('',#5354,#4375,#4376);
#3546=AXIS2_PLACEMENT_3D('',#5359,#4378,#4379);
#3547=AXIS2_PLACEMENT_3D('',#5362,#4381,#4382);
#3548=AXIS2_PLACEMENT_3D('',#5363,#4383,#4384);
#3549=AXIS2_PLACEMENT_3D('',#5368,#4386,#4387);
#3550=AXIS2_PLACEMENT_3D('',#5371,#4389,#4390);
#3551=AXIS2_PLACEMENT_3D('',#5372,#4391,#4392);
#3552=AXIS2_PLACEMENT_3D('',#5373,#4393,#4394);
#3553=AXIS2_PLACEMENT_3D('',#5374,#4395,#4396);
#3554=AXIS2_PLACEMENT_3D('',#5375,#4397,#4398);
#3555=AXIS2_PLACEMENT_3D('',#5376,#4399,#4400);
#3556=AXIS2_PLACEMENT_3D('',#5377,#4401,#4402);
#3557=AXIS2_PLACEMENT_3D('',#5378,#4403,#4404);
#3558=AXIS2_PLACEMENT_3D('',#5380,#4405,#4406);
#3559=AXIS2_PLACEMENT_3D('',#5381,#4407,#4408);
#3560=AXIS2_PLACEMENT_3D('',#5382,#4409,#4410);
#3561=AXIS2_PLACEMENT_3D('',#5383,#4411,#4412);
#3562=AXIS2_PLACEMENT_3D('',#5384,#4413,#4414);
#3563=AXIS2_PLACEMENT_3D('',#5385,#4415,#4416);
#3564=AXIS2_PLACEMENT_3D('',#5386,#4417,#4418);
#3565=AXIS2_PLACEMENT_3D('',#5387,#4419,#4420);
#3566=AXIS2_PLACEMENT_3D('',#5388,#4421,#4422);
#3567=AXIS2_PLACEMENT_3D('',#5389,#4423,#4424);
#3568=AXIS2_PLACEMENT_3D('',#5390,#4425,#4426);
#3569=AXIS2_PLACEMENT_3D('',#5391,#4427,#4428);
#3570=AXIS2_PLACEMENT_3D('',#5392,#4429,#4430);
#3571=AXIS2_PLACEMENT_3D('',#5393,#4431,#4432);
#3572=AXIS2_PLACEMENT_3D('',#5402,#4437,#4438);
#3573=AXIS2_PLACEMENT_3D('',#5408,#4442,#4443);
#3574=AXIS2_PLACEMENT_3D('',#5414,#4447,#4448);
#3575=AXIS2_PLACEMENT_3D('',#5420,#4452,#4453);
#3576=AXIS2_PLACEMENT_3D('',#5426,#4457,#4458);
#3577=AXIS2_PLACEMENT_3D('',#5429,#4461,#4462);
#3578=AXIS2_PLACEMENT_3D('',#5431,#4463,#4464);
#3579=AXIS2_PLACEMENT_3D('',#5432,#4465,#4466);
#3580=AXIS2_PLACEMENT_3D('',#5434,#4468,#4469);
#3581=AXIS2_PLACEMENT_3D('',#5435,#4470,#4471);
#3582=AXIS2_PLACEMENT_3D('',#5436,#4472,#4473);
#3583=AXIS2_PLACEMENT_3D('',#5437,#4474,#4475);
#3584=AXIS2_PLACEMENT_3D('',#5438,#4476,#4477);
#3585=AXIS2_PLACEMENT_3D('',#5439,#4478,#4479);
#3586=AXIS2_PLACEMENT_3D('',#5440,#4480,#4481);
#3587=AXIS2_PLACEMENT_3D('',#5441,#4482,#4483);
#3588=AXIS2_PLACEMENT_3D('',#5442,#4484,#4485);
#3589=AXIS2_PLACEMENT_3D('',#5443,#4486,#4487);
#3590=AXIS2_PLACEMENT_3D('',#5444,#4488,#4489);
#3591=AXIS2_PLACEMENT_3D('',#5445,#4490,#4491);
#3592=AXIS2_PLACEMENT_3D('',#5446,#4492,#4493);
#3593=AXIS2_PLACEMENT_3D('',#5447,#4494,#4495);
#3594=AXIS2_PLACEMENT_3D('',#5448,#4496,#4497);
#3595=AXIS2_PLACEMENT_3D('',#5449,#4498,#4499);
#3596=AXIS2_PLACEMENT_3D('',#5450,#4500,#4501);
#3597=AXIS2_PLACEMENT_3D('',#5451,#4502,#4503);
#3598=AXIS2_PLACEMENT_3D('',#5452,#4504,#4505);
#3599=AXIS2_PLACEMENT_3D('',#5453,#4506,#4507);
#3600=AXIS2_PLACEMENT_3D('',#5454,#4508,#4509);
#3601=AXIS2_PLACEMENT_3D('',#5455,#4510,#4511);
#3602=AXIS2_PLACEMENT_3D('',#5456,#4512,#4513);
#3603=AXIS2_PLACEMENT_3D('',#5457,#4514,#4515);
#3604=AXIS2_PLACEMENT_3D('',#5458,#4516,#4517);
#3605=DIRECTION('axis',(0.,0.,1.));
#3606=DIRECTION('refdir',(1.,0.,0.));
#3607=DIRECTION('axis',(0.,0.,1.));
#3608=DIRECTION('refdir',(1.,0.,0.));
#3609=DIRECTION('axis',(0.,0.,1.));
#3610=DIRECTION('refdir',(1.,0.,0.));
#3611=DIRECTION('center_axis',(0.,0.,1.));
#3612=DIRECTION('ref_axis',(1.,0.,0.));
#3613=DIRECTION('center_axis',(0.,0.,1.));
#3614=DIRECTION('ref_axis',(1.,0.,0.));
#3615=DIRECTION('',(0.,0.,1.));
#3616=DIRECTION('center_axis',(0.,0.,-1.));
#3617=DIRECTION('ref_axis',(1.,0.,0.));
#3618=DIRECTION('center_axis',(0.,0.,1.));
#3619=DIRECTION('ref_axis',(1.,0.,0.));
#3620=DIRECTION('center_axis',(0.,0.,1.));
#3621=DIRECTION('ref_axis',(1.,0.,0.));
#3622=DIRECTION('',(0.,0.,1.));
#3623=DIRECTION('center_axis',(0.,0.,-1.));
#3624=DIRECTION('ref_axis',(1.,0.,0.));
#3625=DIRECTION('center_axis',(0.,1.,0.));
#3626=DIRECTION('ref_axis',(1.,0.,0.));
#3627=DIRECTION('center_axis',(0.,1.,0.));
#3628=DIRECTION('ref_axis',(1.,0.,0.));
#3629=DIRECTION('',(0.,1.,0.));
#3630=DIRECTION('center_axis',(0.,-1.,0.));
#3631=DIRECTION('ref_axis',(1.,0.,0.));
#3632=DIRECTION('center_axis',(-1.,0.,0.));
#3633=DIRECTION('ref_axis',(0.,0.,1.));
#3634=DIRECTION('',(0.,0.,-1.));
#3635=DIRECTION('',(0.,1.,0.));
#3636=DIRECTION('',(0.,0.,1.));
#3637=DIRECTION('',(0.,1.,0.));
#3638=DIRECTION('center_axis',(1.,0.,0.));
#3639=DIRECTION('ref_axis',(0.,0.,-1.));
#3640=DIRECTION('',(0.,0.,1.));
#3641=DIRECTION('',(0.,-1.,0.));
#3642=DIRECTION('',(0.,0.,-1.));
#3643=DIRECTION('',(0.,1.,0.));
#3644=DIRECTION('center_axis',(0.,0.,1.));
#3645=DIRECTION('ref_axis',(1.,0.,0.));
#3646=DIRECTION('',(-1.,0.,0.));
#3647=DIRECTION('',(1.,0.,0.));
#3648=DIRECTION('center_axis',(0.,1.,0.));
#3649=DIRECTION('ref_axis',(1.,0.,0.));
#3650=DIRECTION('',(-1.,0.,0.));
#3651=DIRECTION('center_axis',(0.,0.,1.));
#3652=DIRECTION('ref_axis',(1.,0.,0.));
#3653=DIRECTION('',(-1.,0.,0.));
#3654=DIRECTION('',(0.,-1.,0.));
#3655=DIRECTION('',(1.,0.,0.));
#3656=DIRECTION('',(0.,1.,0.));
#3657=DIRECTION('',(-1.,0.,0.));
#3658=DIRECTION('center_axis',(0.,1.,0.));
#3659=DIRECTION('ref_axis',(-1.,0.,0.));
#3660=DIRECTION('',(-1.,0.,0.));
#3661=DIRECTION('',(0.,0.,1.));
#3662=DIRECTION('',(0.,0.,1.));
#3663=DIRECTION('center_axis',(1.,0.,0.));
#3664=DIRECTION('ref_axis',(0.,1.,0.));
#3665=DIRECTION('',(0.,1.,0.));
#3666=DIRECTION('',(0.,0.,1.));
#3667=DIRECTION('center_axis',(0.,-1.,0.));
#3668=DIRECTION('ref_axis',(1.,0.,0.));
#3669=DIRECTION('',(1.,0.,0.));
#3670=DIRECTION('',(0.,0.,1.));
#3671=DIRECTION('center_axis',(-1.,0.,0.));
#3672=DIRECTION('ref_axis',(0.,-1.,0.));
#3673=DIRECTION('',(0.,-1.,0.));
#3674=DIRECTION('center_axis',(0.,0.,1.));
#3675=DIRECTION('ref_axis',(1.,0.,0.));
#3676=DIRECTION('axis',(0.,0.,1.));
#3677=DIRECTION('refdir',(1.,0.,0.));
#3678=DIRECTION('center_axis',(0.,0.,-1.));
#3679=DIRECTION('ref_axis',(0.,1.,0.));
#3680=DIRECTION('',(0.,1.,0.));
#3681=DIRECTION('',(1.,0.,0.));
#3682=DIRECTION('',(0.,-1.,0.));
#3683=DIRECTION('',(1.,0.,0.));
#3684=DIRECTION('center_axis',(0.,1.,-8.88178419700125E-16));
#3685=DIRECTION('ref_axis',(0.,8.88178419700125E-16,1.));
#3686=DIRECTION('',(0.,8.88178419700125E-16,1.));
#3687=DIRECTION('',(1.,0.,0.));
#3688=DIRECTION('',(0.,-8.88178419700125E-16,-1.));
#3689=DIRECTION('center_axis',(0.,-7.40148683083439E-16,-1.));
#3690=DIRECTION('ref_axis',(0.,1.,-7.40148683083439E-16));
#3691=DIRECTION('',(0.,1.,-7.40148683083439E-16));
#3692=DIRECTION('',(1.,0.,0.));
#3693=DIRECTION('',(0.,-1.,7.40148683083439E-16));
#3694=DIRECTION('center_axis',(0.,-0.707106781186547,-0.707106781186548));
#3695=DIRECTION('ref_axis',(0.,0.707106781186548,-0.707106781186547));
#3696=DIRECTION('',(0.,0.707106781186548,-0.707106781186547));
#3697=DIRECTION('',(1.,0.,0.));
#3698=DIRECTION('',(0.,-0.707106781186548,0.707106781186547));
#3699=DIRECTION('center_axis',(0.,-1.,2.77555756156289E-16));
#3700=DIRECTION('ref_axis',(0.,-2.77555756156289E-16,-1.));
#3701=DIRECTION('',(0.,-2.77555756156289E-16,-1.));
#3702=DIRECTION('',(1.,0.,0.));
#3703=DIRECTION('',(0.,2.77555756156289E-16,1.));
#3704=DIRECTION('center_axis',(0.,-0.707106781186547,0.707106781186548));
#3705=DIRECTION('ref_axis',(0.,-0.707106781186548,-0.707106781186547));
#3706=DIRECTION('',(0.,-0.707106781186548,-0.707106781186547));
#3707=DIRECTION('',(1.,0.,0.));
#3708=DIRECTION('',(0.,0.707106781186548,0.707106781186547));
#3709=DIRECTION('center_axis',(0.,7.40148683083438E-16,1.));
#3710=DIRECTION('ref_axis',(0.,-1.,7.40148683083438E-16));
#3711=DIRECTION('',(0.,-1.,7.40148683083438E-16));
#3712=DIRECTION('',(1.,0.,0.));
#3713=DIRECTION('',(0.,1.,-7.40148683083438E-16));
#3714=DIRECTION('center_axis',(0.,1.,-4.44089209850063E-16));
#3715=DIRECTION('ref_axis',(0.,4.44089209850063E-16,1.));
#3716=DIRECTION('',(0.,4.44089209850063E-16,1.));
#3717=DIRECTION('',(1.,0.,0.));
#3718=DIRECTION('',(0.,-4.44089209850063E-16,-1.));
#3719=DIRECTION('center_axis',(0.,2.41352831440251E-16,1.));
#3720=DIRECTION('ref_axis',(0.,-1.,2.41352831440251E-16));
#3721=DIRECTION('',(0.,-1.,2.41352831440251E-16));
#3722=DIRECTION('',(-1.,0.,0.));
#3723=DIRECTION('',(0.,1.,-2.41352831440251E-16));
#3724=DIRECTION('center_axis',(0.,-1.,2.41352831440251E-16));
#3725=DIRECTION('ref_axis',(0.,-2.41352831440251E-16,-1.));
#3726=DIRECTION('',(0.,-2.41352831440251E-16,-1.));
#3727=DIRECTION('',(1.,0.,0.));
#3728=DIRECTION('',(0.,2.41352831440251E-16,1.));
#3729=DIRECTION('',(1.,0.,0.));
#3730=DIRECTION('center_axis',(0.,0.,-1.));
#3731=DIRECTION('ref_axis',(0.,1.,0.));
#3732=DIRECTION('',(0.,1.,0.));
#3733=DIRECTION('',(1.,0.,0.));
#3734=DIRECTION('',(0.,-1.,0.));
#3735=DIRECTION('center_axis',(0.,-1.,0.));
#3736=DIRECTION('ref_axis',(0.,0.,-1.));
#3737=DIRECTION('',(0.,0.,-1.));
#3738=DIRECTION('',(1.,0.,0.));
#3739=DIRECTION('',(0.,0.,1.));
#3740=DIRECTION('center_axis',(0.,-0.707106781186547,0.707106781186548));
#3741=DIRECTION('ref_axis',(0.,-0.707106781186548,-0.707106781186547));
#3742=DIRECTION('',(0.,-0.707106781186548,-0.707106781186547));
#3743=DIRECTION('',(1.,0.,0.));
#3744=DIRECTION('',(0.,0.707106781186548,0.707106781186547));
#3745=DIRECTION('center_axis',(0.,0.,1.));
#3746=DIRECTION('ref_axis',(0.,-1.,0.));
#3747=DIRECTION('',(0.,-1.,0.));
#3748=DIRECTION('',(1.,0.,0.));
#3749=DIRECTION('',(0.,1.,0.));
#3750=DIRECTION('center_axis',(0.,0.707106781186548,0.707106781186547));
#3751=DIRECTION('ref_axis',(0.,-0.707106781186547,0.707106781186548));
#3752=DIRECTION('',(0.,-0.707106781186547,0.707106781186548));
#3753=DIRECTION('',(1.,0.,0.));
#3754=DIRECTION('',(0.,0.707106781186547,-0.707106781186548));
#3755=DIRECTION('center_axis',(0.,1.,0.));
#3756=DIRECTION('ref_axis',(0.,0.,1.));
#3757=DIRECTION('',(0.,0.,1.));
#3758=DIRECTION('',(1.,0.,0.));
#3759=DIRECTION('',(0.,0.,-1.));
#3760=DIRECTION('center_axis',(0.,0.,-1.));
#3761=DIRECTION('ref_axis',(0.,1.,0.));
#3762=DIRECTION('',(0.,1.,0.));
#3763=DIRECTION('',(1.,0.,0.));
#3764=DIRECTION('',(0.,-1.,0.));
#3765=DIRECTION('center_axis',(0.,1.,-2.41352831440251E-16));
#3766=DIRECTION('ref_axis',(0.,2.41352831440251E-16,1.));
#3767=DIRECTION('',(0.,2.41352831440251E-16,1.));
#3768=DIRECTION('',(-1.,0.,0.));
#3769=DIRECTION('',(0.,-2.41352831440251E-16,-1.));
#3770=DIRECTION('center_axis',(0.,0.,1.));
#3771=DIRECTION('ref_axis',(0.,-1.,0.));
#3772=DIRECTION('',(0.,-1.,0.));
#3773=DIRECTION('',(1.,0.,0.));
#3774=DIRECTION('',(0.,1.,0.));
#3775=DIRECTION('',(1.,0.,0.));
#3776=DIRECTION('center_axis',(0.,-1.,0.));
#3777=DIRECTION('ref_axis',(0.,0.,-1.));
#3778=DIRECTION('',(0.,0.,-1.));
#3779=DIRECTION('',(1.,0.,0.));
#3780=DIRECTION('',(0.,0.,1.));
#3781=DIRECTION('center_axis',(0.,0.,1.));
#3782=DIRECTION('ref_axis',(0.,-1.,0.));
#3783=DIRECTION('',(0.,-1.,0.));
#3784=DIRECTION('',(1.,0.,0.));
#3785=DIRECTION('',(0.,1.,0.));
#3786=DIRECTION('center_axis',(0.,0.707106781186548,0.707106781186548));
#3787=DIRECTION('ref_axis',(0.,-0.707106781186548,0.707106781186548));
#3788=DIRECTION('',(0.,-0.707106781186548,0.707106781186548));
#3789=DIRECTION('',(1.,0.,0.));
#3790=DIRECTION('',(0.,0.707106781186548,-0.707106781186548));
#3791=DIRECTION('center_axis',(0.,1.,0.));
#3792=DIRECTION('ref_axis',(0.,0.,1.));
#3793=DIRECTION('',(0.,0.,1.));
#3794=DIRECTION('',(1.,0.,0.));
#3795=DIRECTION('',(0.,0.,-1.));
#3796=DIRECTION('center_axis',(0.,0.707106781186548,-0.707106781186547));
#3797=DIRECTION('ref_axis',(0.,0.707106781186547,0.707106781186548));
#3798=DIRECTION('',(0.,0.707106781186547,0.707106781186548));
#3799=DIRECTION('',(1.,0.,0.));
#3800=DIRECTION('',(0.,-0.707106781186547,-0.707106781186548));
#3801=DIRECTION('center_axis',(0.,-7.40148683083438E-16,-1.));
#3802=DIRECTION('ref_axis',(0.,1.,-7.40148683083438E-16));
#3803=DIRECTION('',(0.,1.,-7.40148683083438E-16));
#3804=DIRECTION('',(1.,0.,0.));
#3805=DIRECTION('',(0.,-1.,7.40148683083438E-16));
#3806=DIRECTION('center_axis',(0.,-1.,0.));
#3807=DIRECTION('ref_axis',(0.,0.,-1.));
#3808=DIRECTION('',(0.,0.,-1.));
#3809=DIRECTION('',(1.,0.,0.));
#3810=DIRECTION('',(0.,0.,1.));
#3811=DIRECTION('center_axis',(0.,0.,-1.));
#3812=DIRECTION('ref_axis',(0.,1.,0.));
#3813=DIRECTION('',(0.,1.,0.));
#3814=DIRECTION('',(-1.,0.,0.));
#3815=DIRECTION('',(0.,-1.,0.));
#3816=DIRECTION('center_axis',(0.,1.,0.));
#3817=DIRECTION('ref_axis',(0.,0.,1.));
#3818=DIRECTION('',(0.,0.,1.));
#3819=DIRECTION('',(1.,0.,0.));
#3820=DIRECTION('',(0.,0.,-1.));
#3821=DIRECTION('',(1.,0.,0.));
#3822=DIRECTION('center_axis',(0.,0.,1.));
#3823=DIRECTION('ref_axis',(0.,-1.,0.));
#3824=DIRECTION('',(0.,-1.,0.));
#3825=DIRECTION('',(1.,0.,0.));
#3826=DIRECTION('',(0.,1.,0.));
#3827=DIRECTION('center_axis',(0.,1.,0.));
#3828=DIRECTION('ref_axis',(0.,0.,1.));
#3829=DIRECTION('',(0.,0.,1.));
#3830=DIRECTION('',(1.,0.,0.));
#3831=DIRECTION('',(0.,0.,-1.));
#3832=DIRECTION('center_axis',(0.,0.707106781186547,-0.707106781186548));
#3833=DIRECTION('ref_axis',(0.,0.707106781186548,0.707106781186547));
#3834=DIRECTION('',(0.,0.707106781186548,0.707106781186547));
#3835=DIRECTION('',(1.,0.,0.));
#3836=DIRECTION('',(0.,-0.707106781186548,-0.707106781186547));
#3837=DIRECTION('center_axis',(0.,0.,-1.));
#3838=DIRECTION('ref_axis',(0.,1.,0.));
#3839=DIRECTION('',(0.,1.,0.));
#3840=DIRECTION('',(1.,0.,0.));
#3841=DIRECTION('',(0.,-1.,0.));
#3842=DIRECTION('center_axis',(0.,-0.707106781186547,-0.707106781186548));
#3843=DIRECTION('ref_axis',(0.,0.707106781186548,-0.707106781186547));
#3844=DIRECTION('',(0.,0.707106781186548,-0.707106781186547));
#3845=DIRECTION('',(1.,0.,0.));
#3846=DIRECTION('',(0.,-0.707106781186548,0.707106781186547));
#3847=DIRECTION('center_axis',(0.,-1.,0.));
#3848=DIRECTION('ref_axis',(0.,0.,-1.));
#3849=DIRECTION('',(0.,0.,-1.));
#3850=DIRECTION('',(1.,0.,0.));
#3851=DIRECTION('',(0.,0.,1.));
#3852=DIRECTION('center_axis',(0.,0.,1.));
#3853=DIRECTION('ref_axis',(0.,-1.,0.));
#3854=DIRECTION('',(0.,-1.,0.));
#3855=DIRECTION('',(1.,0.,0.));
#3856=DIRECTION('',(0.,1.,0.));
#3857=DIRECTION('center_axis',(0.,-1.,0.));
#3858=DIRECTION('ref_axis',(0.,0.,-1.));
#3859=DIRECTION('',(0.,0.,-1.));
#3860=DIRECTION('',(-1.,0.,0.));
#3861=DIRECTION('',(0.,0.,1.));
#3862=DIRECTION('center_axis',(1.,0.,0.));
#3863=DIRECTION('ref_axis',(0.,0.,-1.));
#3864=DIRECTION('center_axis',(1.,0.,0.));
#3865=DIRECTION('ref_axis',(0.,0.,-1.));
#3866=DIRECTION('',(1.,0.,0.));
#3867=DIRECTION('center_axis',(-1.,0.,0.));
#3868=DIRECTION('ref_axis',(0.,0.,-1.));
#3869=DIRECTION('center_axis',(0.,1.,0.));
#3870=DIRECTION('ref_axis',(0.,0.,1.));
#3871=DIRECTION('',(0.,0.,1.));
#3872=DIRECTION('',(1.,0.,0.));
#3873=DIRECTION('',(0.,0.,1.));
#3874=DIRECTION('center_axis',(0.,1.,0.));
#3875=DIRECTION('ref_axis',(0.,0.,1.));
#3876=DIRECTION('',(0.,0.,1.));
#3877=DIRECTION('',(1.,0.,0.));
#3878=DIRECTION('',(0.,0.,1.));
#3879=DIRECTION('center_axis',(0.,0.,-1.));
#3880=DIRECTION('ref_axis',(0.,1.,0.));
#3881=DIRECTION('',(0.,1.,0.));
#3882=DIRECTION('',(0.,1.,0.));
#3883=DIRECTION('center_axis',(0.,0.,-1.));
#3884=DIRECTION('ref_axis',(0.,1.,0.));
#3885=DIRECTION('',(0.,1.,0.));
#3886=DIRECTION('',(1.,0.,0.));
#3887=DIRECTION('',(0.,1.,0.));
#3888=DIRECTION('center_axis',(0.,-1.,0.));
#3889=DIRECTION('ref_axis',(0.,0.,-1.));
#3890=DIRECTION('',(0.,0.,-1.));
#3891=DIRECTION('',(0.,0.,-1.));
#3892=DIRECTION('center_axis',(0.,-1.,0.));
#3893=DIRECTION('ref_axis',(0.,0.,-1.));
#3894=DIRECTION('',(0.,0.,-1.));
#3895=DIRECTION('',(1.,0.,0.));
#3896=DIRECTION('',(0.,0.,-1.));
#3897=DIRECTION('center_axis',(0.,0.,1.));
#3898=DIRECTION('ref_axis',(0.,-1.,0.));
#3899=DIRECTION('',(0.,-1.,0.));
#3900=DIRECTION('',(0.,-1.,0.));
#3901=DIRECTION('center_axis',(0.,0.,1.));
#3902=DIRECTION('ref_axis',(0.,-1.,0.));
#3903=DIRECTION('',(0.,-1.,0.));
#3904=DIRECTION('',(0.,-1.,0.));
#3905=DIRECTION('center_axis',(1.,0.,0.));
#3906=DIRECTION('ref_axis',(0.,0.,-1.));
#3907=DIRECTION('center_axis',(1.,0.,0.));
#3908=DIRECTION('ref_axis',(0.,0.,-1.));
#3909=DIRECTION('axis',(0.,0.,1.));
#3910=DIRECTION('refdir',(1.,0.,0.));
#3911=DIRECTION('center_axis',(0.,0.,1.));
#3912=DIRECTION('ref_axis',(1.,0.,0.));
#3913=DIRECTION('',(1.,0.,0.));
#3914=DIRECTION('',(0.,-1.,0.));
#3915=DIRECTION('',(-1.,0.,0.));
#3916=DIRECTION('',(0.,1.,0.));
#3917=DIRECTION('center_axis',(0.,1.,0.));
#3918=DIRECTION('ref_axis',(-1.,0.,0.));
#3919=DIRECTION('',(0.,0.,1.));
#3920=DIRECTION('',(-1.,0.,0.));
#3921=DIRECTION('',(0.,0.,1.));
#3922=DIRECTION('center_axis',(0.,0.,1.));
#3923=DIRECTION('ref_axis',(1.,0.,0.));
#3924=DIRECTION('',(0.,-1.,0.));
#3925=DIRECTION('',(1.,0.,0.));
#3926=DIRECTION('',(0.,1.,0.));
#3927=DIRECTION('center_axis',(0.,0.,-1.));
#3928=DIRECTION('ref_axis',(1.,0.,0.));
#3929=DIRECTION('center_axis',(-1.,0.,0.));
#3930=DIRECTION('ref_axis',(0.,-1.,0.));
#3931=DIRECTION('',(0.,0.,1.));
#3932=DIRECTION('',(0.,0.707106781186548,0.707106781186548));
#3933=DIRECTION('',(0.,-1.,0.));
#3934=DIRECTION('',(0.,0.707106781186548,-0.707106781186548));
#3935=DIRECTION('',(0.,0.,1.));
#3936=DIRECTION('',(0.,-1.,0.));
#3937=DIRECTION('',(0.,0.,1.));
#3938=DIRECTION('center_axis',(0.,-1.,0.));
#3939=DIRECTION('ref_axis',(1.,0.,0.));
#3940=DIRECTION('',(1.,0.,0.));
#3941=DIRECTION('',(0.,0.,1.));
#3942=DIRECTION('center_axis',(0.,0.,1.));
#3943=DIRECTION('ref_axis',(1.,0.,0.));
#3944=DIRECTION('',(-1.,0.,0.));
#3945=DIRECTION('',(0.,1.,0.));
#3946=DIRECTION('center_axis',(1.,0.,0.));
#3947=DIRECTION('ref_axis',(0.,1.,0.));
#3948=DIRECTION('',(0.,0.,1.));
#3949=DIRECTION('',(0.,-0.707106781186548,0.707106781186548));
#3950=DIRECTION('',(0.,1.,0.));
#3951=DIRECTION('',(0.,-0.707106781186548,-0.707106781186548));
#3952=DIRECTION('',(0.,0.,1.));
#3953=DIRECTION('center_axis',(0.,-1.,0.));
#3954=DIRECTION('ref_axis',(1.,0.,0.));
#3955=DIRECTION('',(-1.,0.,0.));
#3956=DIRECTION('center_axis',(0.,-0.707106781186548,-0.707106781186548));
#3957=DIRECTION('ref_axis',(-1.,0.,0.));
#3958=DIRECTION('',(1.,0.,0.));
#3959=DIRECTION('center_axis',(0.,0.707106781186548,0.707106781186548));
#3960=DIRECTION('ref_axis',(0.,0.707106781186547,-0.707106781186547));
#3961=DIRECTION('',(1.,0.,0.));
#3962=DIRECTION('center_axis',(0.,0.,1.));
#3963=DIRECTION('ref_axis',(1.,0.,0.));
#3964=DIRECTION('center_axis',(0.,0.,-1.));
#3965=DIRECTION('ref_axis',(1.,0.,0.));
#3966=DIRECTION('',(0.,0.,1.));
#3967=DIRECTION('center_axis',(0.,0.,-1.));
#3968=DIRECTION('ref_axis',(1.,0.,0.));
#3969=DIRECTION('center_axis',(0.,-0.707106781186548,0.707106781186548));
#3970=DIRECTION('ref_axis',(0.,0.707106781186547,0.707106781186547));
#3971=DIRECTION('center_axis',(0.,0.,-1.));
#3972=DIRECTION('ref_axis',(1.,0.,0.));
#3973=DIRECTION('center_axis',(0.,0.,1.));
#3974=DIRECTION('ref_axis',(1.,0.,0.));
#3975=DIRECTION('',(-1.,0.,0.));
#3976=DIRECTION('center_axis',(0.,0.,1.));
#3977=DIRECTION('ref_axis',(1.,0.,0.));
#3978=DIRECTION('',(-1.,0.,0.));
#3979=DIRECTION('center_axis',(0.,0.707106781186548,-0.707106781186548));
#3980=DIRECTION('ref_axis',(-1.,0.,0.));
#3981=DIRECTION('',(1.,0.,0.));
#3982=DIRECTION('center_axis',(0.,1.,0.));
#3983=DIRECTION('ref_axis',(-1.,0.,0.));
#3984=DIRECTION('axis',(0.,0.,1.));
#3985=DIRECTION('refdir',(1.,0.,0.));
#3986=DIRECTION('center_axis',(0.,1.,0.));
#3987=DIRECTION('ref_axis',(1.,0.,0.));
#3988=DIRECTION('center_axis',(0.,1.,0.));
#3989=DIRECTION('ref_axis',(1.,0.,0.));
#3990=DIRECTION('',(0.707106781186548,-0.707106781186547,-8.65956056235494E-17));
#3991=DIRECTION('center_axis',(0.,-1.,0.));
#3992=DIRECTION('ref_axis',(1.,0.,0.));
#3993=DIRECTION('center_axis',(0.,1.,0.));
#3994=DIRECTION('ref_axis',(1.,0.,0.));
#3995=DIRECTION('',(0.,-1.,0.));
#3996=DIRECTION('center_axis',(0.,-1.,0.));
#3997=DIRECTION('ref_axis',(1.,0.,0.));
#3998=DIRECTION('center_axis',(0.,1.,0.));
#3999=DIRECTION('ref_axis',(1.,0.,0.));
#4000=DIRECTION('center_axis',(0.,1.,0.));
#4001=DIRECTION('ref_axis',(1.,0.,0.));
#4002=DIRECTION('center_axis',(0.,1.,0.));
#4003=DIRECTION('ref_axis',(1.,0.,0.));
#4004=DIRECTION('',(0.,-1.,0.));
#4005=DIRECTION('center_axis',(0.,1.,0.));
#4006=DIRECTION('ref_axis',(1.,0.,0.));
#4007=DIRECTION('center_axis',(0.,1.,0.));
#4008=DIRECTION('ref_axis',(1.,0.,0.));
#4009=DIRECTION('axis',(0.,0.,1.));
#4010=DIRECTION('refdir',(1.,0.,0.));
#4011=DIRECTION('center_axis',(0.866025403784439,0.,-0.5));
#4012=DIRECTION('ref_axis',(0.5,0.,0.866025403784439));
#4013=DIRECTION('',(-0.5,0.,-0.866025403784439));
#4014=DIRECTION('',(0.,-1.,0.));
#4015=DIRECTION('',(0.5,0.,0.866025403784439));
#4016=DIRECTION('',(0.,-1.,0.));
#4017=DIRECTION('center_axis',(1.20185167898973E-16,0.,-1.));
#4018=DIRECTION('ref_axis',(1.,0.,1.20185167898973E-16));
#4019=DIRECTION('',(-1.,0.,-1.20185167898973E-16));
#4020=DIRECTION('',(0.,-1.,0.));
#4021=DIRECTION('',(1.,0.,1.20185167898973E-16));
#4022=DIRECTION('center_axis',(-0.866025403784439,0.,-0.5));
#4023=DIRECTION('ref_axis',(0.5,0.,-0.866025403784439));
#4024=DIRECTION('',(-0.5,0.,0.866025403784439));
#4025=DIRECTION('',(0.,-1.,0.));
#4026=DIRECTION('',(0.5,0.,-0.866025403784439));
#4027=DIRECTION('center_axis',(-0.866025403784439,0.,0.5));
#4028=DIRECTION('ref_axis',(-0.5,0.,-0.866025403784439));
#4029=DIRECTION('',(0.5,0.,0.866025403784439));
#4030=DIRECTION('',(0.,-1.,0.));
#4031=DIRECTION('',(-0.5,0.,-0.866025403784439));
#4032=DIRECTION('center_axis',(-2.40370335797945E-16,0.,1.));
#4033=DIRECTION('ref_axis',(-1.,0.,-2.40370335797945E-16));
#4034=DIRECTION('',(1.,0.,2.40370335797945E-16));
#4035=DIRECTION('',(0.,-1.,0.));
#4036=DIRECTION('',(-1.,0.,-2.40370335797945E-16));
#4037=DIRECTION('center_axis',(0.866025403784439,0.,0.5));
#4038=DIRECTION('ref_axis',(-0.5,0.,0.866025403784439));
#4039=DIRECTION('',(0.5,0.,-0.866025403784439));
#4040=DIRECTION('',(-0.5,0.,0.866025403784439));
#4041=DIRECTION('center_axis',(0.,1.,0.));
#4042=DIRECTION('ref_axis',(1.,0.,0.));
#4043=DIRECTION('center_axis',(0.,-1.,0.));
#4044=DIRECTION('ref_axis',(0.,0.,-1.));
#4045=DIRECTION('center_axis',(0.,1.,0.));
#4046=DIRECTION('ref_axis',(1.,0.,0.));
#4047=DIRECTION('center_axis',(0.,1.,0.));
#4048=DIRECTION('ref_axis',(1.,0.,0.));
#4049=DIRECTION('center_axis',(0.,1.,0.));
#4050=DIRECTION('ref_axis',(0.,0.,1.));
#4051=DIRECTION('center_axis',(0.,-1.,0.));
#4052=DIRECTION('ref_axis',(1.,0.,0.));
#4053=DIRECTION('center_axis',(0.,-1.,0.));
#4054=DIRECTION('ref_axis',(1.,0.,0.));
#4055=DIRECTION('center_axis',(0.,-1.,0.));
#4056=DIRECTION('ref_axis',(1.,0.,0.));
#4057=DIRECTION('',(0.707106781186548,0.707106781186547,8.65956056235493E-17));
#4058=DIRECTION('center_axis',(0.,-1.,0.));
#4059=DIRECTION('ref_axis',(1.,0.,0.));
#4060=DIRECTION('center_axis',(0.,-1.,0.));
#4061=DIRECTION('ref_axis',(1.,0.,0.));
#4062=DIRECTION('',(0.,1.,0.));
#4063=DIRECTION('center_axis',(0.,1.,0.));
#4064=DIRECTION('ref_axis',(1.,0.,0.));
#4065=DIRECTION('center_axis',(0.,-1.,0.));
#4066=DIRECTION('ref_axis',(1.,0.,0.));
#4067=DIRECTION('',(-0.707106781186547,0.707106781186548,-8.65956056235493E-17));
#4068=DIRECTION('center_axis',(0.,-1.,0.));
#4069=DIRECTION('ref_axis',(0.,0.,-1.));
#4070=DIRECTION('center_axis',(0.,-1.,0.));
#4071=DIRECTION('ref_axis',(1.,0.,0.));
#4072=DIRECTION('center_axis',(0.,1.,0.));
#4073=DIRECTION('ref_axis',(1.,0.,0.));
#4074=DIRECTION('center_axis',(0.,1.,0.));
#4075=DIRECTION('ref_axis',(1.,0.,0.));
#4076=DIRECTION('',(-0.447213595499958,0.894427190999916,-5.47678698264203E-17));
#4077=DIRECTION('center_axis',(0.,-1.,0.));
#4078=DIRECTION('ref_axis',(1.,0.,0.));
#4079=DIRECTION('',(0.,1.,0.));
#4080=DIRECTION('axis',(0.,0.,1.));
#4081=DIRECTION('refdir',(1.,0.,0.));
#4082=DIRECTION('axis',(0.,0.,1.));
#4083=DIRECTION('refdir',(1.,0.,0.));
#4084=DIRECTION('axis',(0.,0.,1.));
#4085=DIRECTION('refdir',(1.,0.,0.));
#4086=DIRECTION('center_axis',(0.,1.,0.));
#4087=DIRECTION('ref_axis',(1.,0.,0.));
#4088=DIRECTION('center_axis',(0.,1.,0.));
#4089=DIRECTION('ref_axis',(1.,0.,0.));
#4090=DIRECTION('',(0.,1.,0.));
#4091=DIRECTION('center_axis',(0.,-1.,0.));
#4092=DIRECTION('ref_axis',(1.,0.,0.));
#4093=DIRECTION('center_axis',(0.,1.,0.));
#4094=DIRECTION('ref_axis',(1.,0.,0.));
#4095=DIRECTION('center_axis',(0.,1.,0.));
#4096=DIRECTION('ref_axis',(1.,0.,0.));
#4097=DIRECTION('',(0.,1.,0.));
#4098=DIRECTION('center_axis',(0.,-1.,0.));
#4099=DIRECTION('ref_axis',(1.,0.,0.));
#4100=DIRECTION('center_axis',(0.,1.,0.));
#4101=DIRECTION('ref_axis',(1.,0.,0.));
#4102=DIRECTION('',(0.,-1.,0.));
#4103=DIRECTION('center_axis',(0.,1.,0.));
#4104=DIRECTION('ref_axis',(1.,0.,0.));
#4105=DIRECTION('',(0.,1.,0.));
#4106=DIRECTION('center_axis',(0.,1.,0.));
#4107=DIRECTION('ref_axis',(1.,0.,0.));
#4108=DIRECTION('center_axis',(0.,0.,-1.));
#4109=DIRECTION('ref_axis',(-1.,0.,0.));
#4110=DIRECTION('',(1.,0.,0.));
#4111=DIRECTION('',(0.,-1.,0.));
#4112=DIRECTION('',(-1.,0.,0.));
#4113=DIRECTION('center_axis',(0.,1.,0.));
#4114=DIRECTION('ref_axis',(1.,0.,0.));
#4115=DIRECTION('',(-1.,0.,0.));
#4116=DIRECTION('center_axis',(0.,1.,0.));
#4117=DIRECTION('ref_axis',(1.,0.,0.));
#4118=DIRECTION('center_axis',(0.,0.,1.));
#4119=DIRECTION('ref_axis',(1.,0.,0.));
#4120=DIRECTION('',(1.,0.,0.));
#4121=DIRECTION('',(0.,1.,0.));
#4122=DIRECTION('center_axis',(0.,1.,0.));
#4123=DIRECTION('ref_axis',(-1.,0.,-1.22464679914735E-16));
#4124=DIRECTION('center_axis',(0.,1.,0.));
#4125=DIRECTION('ref_axis',(1.,0.,0.));
#4126=DIRECTION('center_axis',(0.,1.,0.));
#4127=DIRECTION('ref_axis',(1.,0.,0.));
#4128=DIRECTION('axis',(0.,0.,1.));
#4129=DIRECTION('refdir',(1.,0.,0.));
#4130=DIRECTION('center_axis',(0.,-1.,0.));
#4131=DIRECTION('ref_axis',(1.,0.,0.));
#4132=DIRECTION('center_axis',(0.,1.,0.));
#4133=DIRECTION('ref_axis',(1.,0.,0.));
#4134=DIRECTION('',(0.,1.,0.));
#4135=DIRECTION('center_axis',(0.,-1.,0.));
#4136=DIRECTION('ref_axis',(1.,0.,0.));
#4137=DIRECTION('center_axis',(0.,1.,0.));
#4138=DIRECTION('ref_axis',(1.,0.,0.));
#4139=DIRECTION('center_axis',(0.,-1.,0.));
#4140=DIRECTION('ref_axis',(1.,0.,0.));
#4141=DIRECTION('',(-0.707106781186549,0.707106781186546,-8.65956056235496E-17));
#4142=DIRECTION('center_axis',(0.,-1.,0.));
#4143=DIRECTION('ref_axis',(0.,0.,-1.));
#4144=DIRECTION('center_axis',(0.,-1.,0.));
#4145=DIRECTION('ref_axis',(1.,0.,0.));
#4146=DIRECTION('center_axis',(0.,1.,0.));
#4147=DIRECTION('ref_axis',(1.,0.,0.));
#4148=DIRECTION('',(-0.866025403784439,-0.5,-1.06057523872491E-16));
#4149=DIRECTION('center_axis',(1.4792020664489E-16,0.,-1.));
#4150=DIRECTION('ref_axis',(-1.,0.,-1.4792020664489E-16));
#4151=DIRECTION('',(0.,1.,0.));
#4152=DIRECTION('',(-1.,0.,-1.4792020664489E-16));
#4153=DIRECTION('',(0.,1.,0.));
#4154=DIRECTION('center_axis',(0.866025403784439,0.,-0.5));
#4155=DIRECTION('ref_axis',(-0.5,0.,-0.866025403784439));
#4156=DIRECTION('',(0.,1.,0.));
#4157=DIRECTION('',(-0.5,0.,-0.866025403784439));
#4158=DIRECTION('center_axis',(0.866025403784439,0.,0.5));
#4159=DIRECTION('ref_axis',(0.5,0.,-0.866025403784439));
#4160=DIRECTION('',(0.,1.,0.));
#4161=DIRECTION('',(0.5,0.,-0.866025403784439));
#4162=DIRECTION('center_axis',(-2.95840413289779E-16,0.,1.));
#4163=DIRECTION('ref_axis',(1.,0.,2.95840413289779E-16));
#4164=DIRECTION('',(0.,1.,0.));
#4165=DIRECTION('',(1.,0.,2.95840413289779E-16));
#4166=DIRECTION('center_axis',(-0.866025403784439,0.,0.5));
#4167=DIRECTION('ref_axis',(0.5,0.,0.866025403784439));
#4168=DIRECTION('',(0.,1.,0.));
#4169=DIRECTION('',(0.5,0.,0.866025403784439));
#4170=DIRECTION('center_axis',(-0.866025403784439,0.,-0.5));
#4171=DIRECTION('ref_axis',(-0.5,0.,0.866025403784439));
#4172=DIRECTION('',(-0.5,0.,0.866025403784439));
#4173=DIRECTION('center_axis',(0.,1.,0.));
#4174=DIRECTION('ref_axis',(0.,0.,1.));
#4175=DIRECTION('center_axis',(0.,1.,0.));
#4176=DIRECTION('ref_axis',(1.,0.,0.));
#4177=DIRECTION('',(0.,0.,1.));
#4178=DIRECTION('',(1.,0.,0.));
#4179=DIRECTION('',(0.,0.,1.));
#4180=DIRECTION('',(1.,0.,0.));
#4181=DIRECTION('',(0.,0.,1.));
#4182=DIRECTION('',(1.,0.,0.));
#4183=DIRECTION('',(0.,-1.,2.22044604925031E-16));
#4184=DIRECTION('',(1.,0.,0.));
#4185=DIRECTION('',(0.,-1.,2.22044604925031E-16));
#4186=DIRECTION('',(1.,0.,0.));
#4187=DIRECTION('',(0.,0.,1.));
#4188=DIRECTION('',(1.,0.,0.));
#4189=DIRECTION('',(0.,-1.,2.22044604925031E-16));
#4190=DIRECTION('',(1.,0.,0.));
#4191=DIRECTION('',(0.,-1.,2.22044604925031E-16));
#4192=DIRECTION('',(1.,0.,0.));
#4193=DIRECTION('',(0.,0.,1.));
#4194=DIRECTION('',(-1.,1.22464679914735E-16,0.));
#4195=DIRECTION('axis',(0.,0.,1.));
#4196=DIRECTION('refdir',(1.,0.,0.));
#4197=DIRECTION('axis',(0.,0.,1.));
#4198=DIRECTION('refdir',(1.,0.,0.));
#4199=DIRECTION('center_axis',(0.,1.,0.));
#4200=DIRECTION('ref_axis',(1.,0.,0.));
#4201=DIRECTION('center_axis',(0.,1.,0.));
#4202=DIRECTION('ref_axis',(1.,0.,0.));
#4203=DIRECTION('',(0.,1.,0.));
#4204=DIRECTION('center_axis',(0.,-1.,0.));
#4205=DIRECTION('ref_axis',(1.,0.,0.));
#4206=DIRECTION('center_axis',(0.,1.,0.));
#4207=DIRECTION('ref_axis',(1.,0.,0.));
#4208=DIRECTION('center_axis',(0.,1.,0.));
#4209=DIRECTION('ref_axis',(1.,0.,0.));
#4210=DIRECTION('',(0.,1.,0.));
#4211=DIRECTION('center_axis',(0.,-1.,0.));
#4212=DIRECTION('ref_axis',(1.,0.,0.));
#4213=DIRECTION('center_axis',(0.,1.,0.));
#4214=DIRECTION('ref_axis',(1.,0.,0.));
#4215=DIRECTION('center_axis',(0.,1.,0.));
#4216=DIRECTION('ref_axis',(1.,0.,0.));
#4217=DIRECTION('',(0.,1.,0.));
#4218=DIRECTION('center_axis',(0.,-1.,0.));
#4219=DIRECTION('ref_axis',(1.,0.,0.));
#4220=DIRECTION('center_axis',(0.,1.,0.));
#4221=DIRECTION('ref_axis',(1.,0.,0.));
#4222=DIRECTION('center_axis',(0.,1.,0.));
#4223=DIRECTION('ref_axis',(1.,0.,0.));
#4224=DIRECTION('',(0.,1.,0.));
#4225=DIRECTION('center_axis',(0.,-1.,0.));
#4226=DIRECTION('ref_axis',(1.,0.,0.));
#4227=DIRECTION('center_axis',(0.,1.,0.));
#4228=DIRECTION('ref_axis',(1.,0.,0.));
#4229=DIRECTION('center_axis',(0.,1.,0.));
#4230=DIRECTION('ref_axis',(1.,0.,0.));
#4231=DIRECTION('',(0.,1.,0.));
#4232=DIRECTION('center_axis',(0.,-1.,0.));
#4233=DIRECTION('ref_axis',(1.,0.,0.));
#4234=DIRECTION('center_axis',(0.,0.,-1.));
#4235=DIRECTION('ref_axis',(-1.,0.,0.));
#4236=DIRECTION('',(0.,-1.,0.));
#4237=DIRECTION('',(-1.,0.,0.));
#4238=DIRECTION('',(0.,1.,0.));
#4239=DIRECTION('',(1.,0.,0.));
#4240=DIRECTION('center_axis',(-1.,0.,0.));
#4241=DIRECTION('ref_axis',(0.,0.,1.));
#4242=DIRECTION('',(0.,0.,-1.));
#4243=DIRECTION('',(0.,1.,0.));
#4244=DIRECTION('',(0.,0.,1.));
#4245=DIRECTION('',(0.,1.,0.));
#4246=DIRECTION('center_axis',(0.,0.,-1.));
#4247=DIRECTION('ref_axis',(-1.,0.,0.));
#4248=DIRECTION('',(0.,1.,0.));
#4249=DIRECTION('',(1.,0.,0.));
#4250=DIRECTION('',(-1.,0.,0.));
#4251=DIRECTION('center_axis',(1.,0.,0.));
#4252=DIRECTION('ref_axis',(0.,0.,-1.));
#4253=DIRECTION('',(0.,0.,1.));
#4254=DIRECTION('',(0.,0.,-1.));
#4255=DIRECTION('',(0.,1.,0.));
#4256=DIRECTION('center_axis',(0.,0.,1.));
#4257=DIRECTION('ref_axis',(1.,0.,0.));
#4258=DIRECTION('',(-1.,0.,0.));
#4259=DIRECTION('',(1.,0.,0.));
#4260=DIRECTION('center_axis',(-1.,0.,0.));
#4261=DIRECTION('ref_axis',(0.,0.,1.));
#4262=DIRECTION('',(0.,0.,1.));
#4263=DIRECTION('',(0.,1.,0.));
#4264=DIRECTION('',(0.,0.,-1.));
#4265=DIRECTION('center_axis',(0.,1.,0.));
#4266=DIRECTION('ref_axis',(1.,0.,0.));
#4267=DIRECTION('',(0.,0.,-1.));
#4268=DIRECTION('center_axis',(0.,1.,0.));
#4269=DIRECTION('ref_axis',(1.,0.,0.));
#4270=DIRECTION('center_axis',(1.,0.,0.));
#4271=DIRECTION('ref_axis',(0.,0.,-1.));
#4272=DIRECTION('',(0.,0.,1.));
#4273=DIRECTION('',(0.,-1.,0.));
#4274=DIRECTION('center_axis',(0.,1.,0.));
#4275=DIRECTION('ref_axis',(-1.83697019872103E-16,0.,-1.));
#4276=DIRECTION('center_axis',(0.,1.,0.));
#4277=DIRECTION('ref_axis',(1.,0.,0.));
#4278=DIRECTION('center_axis',(0.,1.,0.));
#4279=DIRECTION('ref_axis',(1.,0.,0.));
#4280=DIRECTION('axis',(0.,0.,1.));
#4281=DIRECTION('refdir',(1.,0.,0.));
#4282=DIRECTION('center_axis',(0.,1.,0.));
#4283=DIRECTION('ref_axis',(1.,0.,0.));
#4284=DIRECTION('center_axis',(0.,-1.,0.));
#4285=DIRECTION('ref_axis',(1.,0.,0.));
#4286=DIRECTION('',(0.,-1.,0.));
#4287=DIRECTION('center_axis',(0.,-1.,0.));
#4288=DIRECTION('ref_axis',(1.,0.,0.));
#4289=DIRECTION('center_axis',(0.,1.,0.));
#4290=DIRECTION('ref_axis',(1.,0.,0.));
#4291=DIRECTION('center_axis',(0.,1.,0.));
#4292=DIRECTION('ref_axis',(1.,0.,0.));
#4293=DIRECTION('',(0.,-1.,0.));
#4294=DIRECTION('center_axis',(0.,1.,0.));
#4295=DIRECTION('ref_axis',(1.,0.,0.));
#4296=DIRECTION('center_axis',(0.,1.,0.));
#4297=DIRECTION('ref_axis',(1.,0.,0.));
#4298=DIRECTION('center_axis',(0.,1.,0.));
#4299=DIRECTION('ref_axis',(1.,0.,0.));
#4300=DIRECTION('axis',(0.,0.,1.));
#4301=DIRECTION('refdir',(1.,0.,0.));
#4302=DIRECTION('center_axis',(0.,1.,0.));
#4303=DIRECTION('ref_axis',(1.,0.,0.));
#4304=DIRECTION('',(0.866025403784439,-0.5,1.06057523872491E-16));
#4305=DIRECTION('center_axis',(0.,-1.,0.));
#4306=DIRECTION('ref_axis',(1.,0.,0.));
#4307=DIRECTION('center_axis',(0.,-1.,0.));
#4308=DIRECTION('ref_axis',(1.,0.,0.));
#4309=DIRECTION('center_axis',(0.,1.,0.));
#4310=DIRECTION('ref_axis',(1.,0.,0.));
#4311=DIRECTION('',(-0.866025403784439,-0.5,-1.06057523872491E-16));
#4312=DIRECTION('center_axis',(1.4792020664489E-16,0.,-1.));
#4313=DIRECTION('ref_axis',(-1.,0.,-1.4792020664489E-16));
#4314=DIRECTION('',(0.,1.,0.));
#4315=DIRECTION('',(0.,1.,0.));
#4316=DIRECTION('center_axis',(-0.866025403784439,0.,-0.5));
#4317=DIRECTION('ref_axis',(-0.5,0.,0.866025403784439));
#4318=DIRECTION('',(0.,1.,0.));
#4319=DIRECTION('center_axis',(-0.866025403784439,0.,0.5));
#4320=DIRECTION('ref_axis',(0.5,0.,0.866025403784439));
#4321=DIRECTION('',(0.,1.,0.));
#4322=DIRECTION('center_axis',(0.,1.,0.));
#4323=DIRECTION('ref_axis',(1.,0.,0.));
#4324=DIRECTION('center_axis',(0.,1.,0.));
#4325=DIRECTION('ref_axis',(1.,0.,0.));
#4326=DIRECTION('',(0.,-1.,0.));
#4327=DIRECTION('center_axis',(0.,1.,0.));
#4328=DIRECTION('ref_axis',(1.,0.,0.));
#4329=DIRECTION('center_axis',(-2.95840413289779E-16,0.,1.));
#4330=DIRECTION('ref_axis',(1.,0.,2.95840413289779E-16));
#4331=DIRECTION('',(0.,1.,0.));
#4332=DIRECTION('center_axis',(0.866025403784439,0.,-0.5));
#4333=DIRECTION('ref_axis',(-0.5,0.,-0.866025403784439));
#4334=DIRECTION('',(0.,1.,0.));
#4335=DIRECTION('center_axis',(0.866025403784439,0.,0.5));
#4336=DIRECTION('ref_axis',(0.5,0.,-0.866025403784439));
#4337=DIRECTION('center_axis',(0.,1.,0.));
#4338=DIRECTION('ref_axis',(1.,0.,0.));
#4339=DIRECTION('center_axis',(0.,1.,0.));
#4340=DIRECTION('ref_axis',(1.,0.,0.));
#4341=DIRECTION('axis',(0.,0.,1.));
#4342=DIRECTION('refdir',(1.,0.,0.));
#4343=DIRECTION('center_axis',(0.,0.,1.));
#4344=DIRECTION('ref_axis',(1.,0.,0.));
#4345=DIRECTION('',(0.,0.,-1.));
#4346=DIRECTION('center_axis',(0.,0.,-1.));
#4347=DIRECTION('ref_axis',(1.,0.,0.));
#4348=DIRECTION('',(0.,0.,1.));
#4349=DIRECTION('center_axis',(0.,0.,1.));
#4350=DIRECTION('ref_axis',(1.,0.,0.));
#4351=DIRECTION('center_axis',(0.,0.,1.));
#4352=DIRECTION('ref_axis',(-1.,-1.22464679914735E-16,0.));
#4353=DIRECTION('',(0.,0.,1.));
#4354=DIRECTION('center_axis',(0.,0.,1.));
#4355=DIRECTION('ref_axis',(1.,0.,0.));
#4356=DIRECTION('',(0.,0.,-1.));
#4357=DIRECTION('center_axis',(0.,0.,-1.));
#4358=DIRECTION('ref_axis',(1.,0.,0.));
#4359=DIRECTION('center_axis',(0.,0.,1.));
#4360=DIRECTION('ref_axis',(1.,0.,0.));
#4361=DIRECTION('',(0.,0.,-1.));
#4362=DIRECTION('center_axis',(0.,0.,-1.));
#4363=DIRECTION('ref_axis',(1.,0.,0.));
#4364=DIRECTION('',(0.,0.,1.));
#4365=DIRECTION('center_axis',(0.,0.,1.));
#4366=DIRECTION('ref_axis',(1.,0.,0.));
#4367=DIRECTION('center_axis',(0.,0.,1.));
#4368=DIRECTION('ref_axis',(1.,0.,0.));
#4369=DIRECTION('',(0.,0.,-1.));
#4370=DIRECTION('center_axis',(0.,0.,-1.));
#4371=DIRECTION('ref_axis',(1.,0.,0.));
#4372=DIRECTION('',(0.,0.,1.));
#4373=DIRECTION('center_axis',(0.,0.,1.));
#4374=DIRECTION('ref_axis',(1.,0.,0.));
#4375=DIRECTION('center_axis',(0.,0.,1.));
#4376=DIRECTION('ref_axis',(1.,0.,0.));
#4377=DIRECTION('',(0.,0.,-1.));
#4378=DIRECTION('center_axis',(0.,0.,-1.));
#4379=DIRECTION('ref_axis',(1.,0.,0.));
#4380=DIRECTION('',(0.,0.,1.));
#4381=DIRECTION('center_axis',(0.,0.,1.));
#4382=DIRECTION('ref_axis',(1.,0.,0.));
#4383=DIRECTION('center_axis',(0.,0.,1.));
#4384=DIRECTION('ref_axis',(1.,0.,0.));
#4385=DIRECTION('',(0.,0.,-1.));
#4386=DIRECTION('center_axis',(0.,0.,-1.));
#4387=DIRECTION('ref_axis',(1.,0.,0.));
#4388=DIRECTION('',(0.,0.,1.));
#4389=DIRECTION('center_axis',(0.,0.,1.));
#4390=DIRECTION('ref_axis',(1.,0.,0.));
#4391=DIRECTION('center_axis',(0.,0.,1.));
#4392=DIRECTION('ref_axis',(1.,0.,0.));
#4393=DIRECTION('center_axis',(0.,0.,1.));
#4394=DIRECTION('ref_axis',(1.,0.,0.));
#4395=DIRECTION('center_axis',(0.,0.,1.));
#4396=DIRECTION('ref_axis',(1.,0.,0.));
#4397=DIRECTION('center_axis',(0.,0.,1.));
#4398=DIRECTION('ref_axis',(1.,0.,0.));
#4399=DIRECTION('center_axis',(0.,0.,1.));
#4400=DIRECTION('ref_axis',(1.,0.,0.));
#4401=DIRECTION('center_axis',(0.,0.,1.));
#4402=DIRECTION('ref_axis',(1.,0.,0.));
#4403=DIRECTION('center_axis',(0.,0.,1.));
#4404=DIRECTION('ref_axis',(1.,0.,0.));
#4405=DIRECTION('center_axis',(0.,0.,-1.));
#4406=DIRECTION('ref_axis',(1.,0.,0.));
#4407=DIRECTION('center_axis',(0.,0.,1.));
#4408=DIRECTION('ref_axis',(1.,0.,0.));
#4409=DIRECTION('center_axis',(0.,0.,1.));
#4410=DIRECTION('ref_axis',(1.,0.,0.));
#4411=DIRECTION('center_axis',(0.,0.,1.));
#4412=DIRECTION('ref_axis',(1.,0.,0.));
#4413=DIRECTION('center_axis',(0.,0.,1.));
#4414=DIRECTION('ref_axis',(1.,0.,0.));
#4415=DIRECTION('center_axis',(0.,0.,1.));
#4416=DIRECTION('ref_axis',(1.,0.,0.));
#4417=DIRECTION('center_axis',(0.,0.,1.));
#4418=DIRECTION('ref_axis',(1.,0.,0.));
#4419=DIRECTION('center_axis',(0.,0.,1.));
#4420=DIRECTION('ref_axis',(1.,0.,0.));
#4421=DIRECTION('center_axis',(0.,0.,1.));
#4422=DIRECTION('ref_axis',(1.,0.,0.));
#4423=DIRECTION('center_axis',(0.,0.,1.));
#4424=DIRECTION('ref_axis',(1.,0.,0.));
#4425=DIRECTION('center_axis',(0.,0.,1.));
#4426=DIRECTION('ref_axis',(1.,0.,0.));
#4427=DIRECTION('center_axis',(0.,0.,1.));
#4428=DIRECTION('ref_axis',(1.,0.,0.));
#4429=DIRECTION('center_axis',(0.,0.,1.));
#4430=DIRECTION('ref_axis',(1.,0.,0.));
#4431=DIRECTION('center_axis',(0.,1.,0.));
#4432=DIRECTION('ref_axis',(-1.,0.,0.));
#4433=DIRECTION('',(-1.,0.,0.));
#4434=DIRECTION('',(0.,0.,1.));
#4435=DIRECTION('',(-1.,0.,0.));
#4436=DIRECTION('',(0.,0.,1.));
#4437=DIRECTION('center_axis',(-0.866025403784438,0.500000000000001,0.));
#4438=DIRECTION('ref_axis',(-0.500000000000001,-0.866025403784438,0.));
#4439=DIRECTION('',(-0.500000000000001,-0.866025403784438,0.));
#4440=DIRECTION('',(-0.500000000000001,-0.866025403784438,0.));
#4441=DIRECTION('',(0.,0.,1.));
#4442=DIRECTION('center_axis',(-0.866025403784439,-0.5,0.));
#4443=DIRECTION('ref_axis',(0.5,-0.866025403784439,0.));
#4444=DIRECTION('',(0.5,-0.866025403784439,0.));
#4445=DIRECTION('',(0.5,-0.866025403784439,0.));
#4446=DIRECTION('',(0.,0.,1.));
#4447=DIRECTION('center_axis',(0.,-1.,0.));
#4448=DIRECTION('ref_axis',(1.,0.,0.));
#4449=DIRECTION('',(1.,0.,0.));
#4450=DIRECTION('',(1.,0.,0.));
#4451=DIRECTION('',(0.,0.,1.));
#4452=DIRECTION('center_axis',(0.866025403784439,0.5,0.));
#4453=DIRECTION('ref_axis',(-0.5,0.866025403784439,0.));
#4454=DIRECTION('',(-0.5,0.866025403784439,0.));
#4455=DIRECTION('',(0.,0.,1.));
#4456=DIRECTION('',(-0.5,0.866025403784439,0.));
#4457=DIRECTION('center_axis',(0.866025403784439,-0.5,0.));
#4458=DIRECTION('ref_axis',(0.5,0.866025403784439,0.));
#4459=DIRECTION('',(0.5,0.866025403784439,0.));
#4460=DIRECTION('',(0.5,0.866025403784439,0.));
#4461=DIRECTION('center_axis',(0.,0.,1.));
#4462=DIRECTION('ref_axis',(1.,0.,0.));
#4463=DIRECTION('center_axis',(0.,0.,-1.));
#4464=DIRECTION('ref_axis',(1.,0.,0.));
#4465=DIRECTION('center_axis',(0.,0.,1.));
#4466=DIRECTION('ref_axis',(1.,0.,0.));
#4467=DIRECTION('',(0.,0.,-1.));
#4468=DIRECTION('center_axis',(0.,0.,1.));
#4469=DIRECTION('ref_axis',(1.,0.,0.));
#4470=DIRECTION('',(0.,0.,1.));
#4471=DIRECTION('',(1.,0.,0.));
#4472=DIRECTION('',(0.,0.,1.));
#4473=DIRECTION('',(1.,0.,0.));
#4474=DIRECTION('',(0.,0.,1.));
#4475=DIRECTION('',(1.,0.,0.));
#4476=DIRECTION('',(0.,0.,1.));
#4477=DIRECTION('',(1.,0.,0.));
#4478=DIRECTION('',(0.,0.,1.));
#4479=DIRECTION('',(1.,0.,0.));
#4480=DIRECTION('',(0.,1.,2.22044604925031E-16));
#4481=DIRECTION('',(1.,0.,0.));
#4482=DIRECTION('',(0.,0.,1.));
#4483=DIRECTION('',(-1.,1.22464679914735E-16,0.));
#4484=DIRECTION('',(0.,0.,1.));
#4485=DIRECTION('',(1.,0.,0.));
#4486=DIRECTION('',(0.,0.,1.));
#4487=DIRECTION('',(1.,0.,0.));
#4488=DIRECTION('',(0.,0.,1.));
#4489=DIRECTION('',(1.,0.,0.));
#4490=DIRECTION('',(0.,0.,1.));
#4491=DIRECTION('',(1.,0.,0.));
#4492=DIRECTION('',(0.,0.,1.));
#4493=DIRECTION('',(1.,0.,0.));
#4494=DIRECTION('',(0.,1.,2.22044604925031E-16));
#4495=DIRECTION('',(1.,0.,0.));
#4496=DIRECTION('',(0.,0.,1.));
#4497=DIRECTION('',(-1.,1.22464679914735E-16,0.));
#4498=DIRECTION('',(0.,0.,1.));
#4499=DIRECTION('',(1.,0.,0.));
#4500=DIRECTION('',(0.,0.,1.));
#4501=DIRECTION('',(1.,0.,0.));
#4502=DIRECTION('',(0.,0.,1.));
#4503=DIRECTION('',(1.,0.,0.));
#4504=DIRECTION('',(0.,0.,1.));
#4505=DIRECTION('',(1.,0.,0.));
#4506=DIRECTION('',(0.,0.,1.));
#4507=DIRECTION('',(1.,0.,0.));
#4508=DIRECTION('',(0.,1.,2.22044604925031E-16));
#4509=DIRECTION('',(1.,0.,0.));
#4510=DIRECTION('',(0.,0.,1.));
#4511=DIRECTION('',(1.,0.,0.));
#4512=DIRECTION('',(0.,0.,1.));
#4513=DIRECTION('',(1.,0.,0.));
#4514=DIRECTION('',(0.,0.,1.));
#4515=DIRECTION('',(1.,0.,0.));
#4516=DIRECTION('',(0.,0.,1.));
#4517=DIRECTION('',(1.,0.,0.));
#4518=CARTESIAN_POINT('',(0.,0.,0.));
#4519=CARTESIAN_POINT('',(0.,0.,0.));
#4520=CARTESIAN_POINT('',(0.,0.,0.));
#4521=CARTESIAN_POINT('Origin',(2.5,-2.,1.9));
#4522=CARTESIAN_POINT('',(2.225,-2.,2.));
#4523=CARTESIAN_POINT('Origin',(2.5,-2.,2.));
#4524=CARTESIAN_POINT('',(2.225,-2.,2.8));
#4525=CARTESIAN_POINT('',(2.225,-2.,1.9));
#4526=CARTESIAN_POINT('Origin',(2.5,-2.,2.8));
#4527=CARTESIAN_POINT('Origin',(7.5,-2.,1.9));
#4528=CARTESIAN_POINT('',(7.225,-2.,2.));
#4529=CARTESIAN_POINT('Origin',(7.5,-2.,2.));
#4530=CARTESIAN_POINT('',(7.225,-2.,2.8));
#4531=CARTESIAN_POINT('',(7.225,-2.,1.9));
#4532=CARTESIAN_POINT('Origin',(7.5,-2.,2.8));
#4533=CARTESIAN_POINT('Origin',(5.,-0.9,8.));
#4534=CARTESIAN_POINT('',(4.575,-0.8,8.));
#4535=CARTESIAN_POINT('Origin',(5.,-0.8,8.));
#4536=CARTESIAN_POINT('',(4.575,0.,8.));
#4537=CARTESIAN_POINT('',(4.575,-0.9,8.));
#4538=CARTESIAN_POINT('Origin',(5.,0.,8.));
#4539=CARTESIAN_POINT('Origin',(3.5,-0.8,2.8));
#4540=CARTESIAN_POINT('',(3.5,-0.8,9.5));
#4541=CARTESIAN_POINT('',(3.5,-0.8,2.8));
#4542=CARTESIAN_POINT('',(3.5,-0.8,9.5));
#4543=CARTESIAN_POINT('',(3.5,0.,9.5));
#4544=CARTESIAN_POINT('',(3.5,-0.8,9.5));
#4545=CARTESIAN_POINT('',(3.5,0.,2.8));
#4546=CARTESIAN_POINT('',(3.5,0.,9.5));
#4547=CARTESIAN_POINT('',(3.5,-1.15,2.8));
#4548=CARTESIAN_POINT('Origin',(6.5,-0.8,9.5));
#4549=CARTESIAN_POINT('',(6.5,-0.8,2.8));
#4550=CARTESIAN_POINT('',(6.5,-0.8,9.5));
#4551=CARTESIAN_POINT('',(6.5,-0.8,2.8));
#4552=CARTESIAN_POINT('',(6.5,0.,2.8));
#4553=CARTESIAN_POINT('',(6.5,-1.15,2.8));
#4554=CARTESIAN_POINT('',(6.5,0.,9.5));
#4555=CARTESIAN_POINT('',(6.5,0.,2.8));
#4556=CARTESIAN_POINT('',(6.5,-0.8,9.5));
#4557=CARTESIAN_POINT('Origin',(3.5,-0.8,9.5));
#4558=CARTESIAN_POINT('',(6.5,-0.8,9.5));
#4559=CARTESIAN_POINT('',(6.5,0.,9.5));
#4560=CARTESIAN_POINT('Origin',(5.,-0.8,6.15));
#4561=CARTESIAN_POINT('',(5.,-0.8,2.8));
#4562=CARTESIAN_POINT('Origin',(5.,-1.5,2.8));
#4563=CARTESIAN_POINT('',(1.5,0.,2.8));
#4564=CARTESIAN_POINT('',(8.5,0.,2.8));
#4565=CARTESIAN_POINT('',(1.5,-3.,2.8));
#4566=CARTESIAN_POINT('',(1.5,0.,2.8));
#4567=CARTESIAN_POINT('',(8.5,-3.,2.8));
#4568=CARTESIAN_POINT('',(1.5,-3.,2.8));
#4569=CARTESIAN_POINT('',(8.5,0.,2.8));
#4570=CARTESIAN_POINT('',(8.5,-3.,2.8));
#4571=CARTESIAN_POINT('',(8.5,0.,2.8));
#4572=CARTESIAN_POINT('Origin',(8.5,0.,2.));
#4573=CARTESIAN_POINT('',(8.5,0.,2.));
#4574=CARTESIAN_POINT('',(1.5,0.,2.));
#4575=CARTESIAN_POINT('',(8.5,0.,2.));
#4576=CARTESIAN_POINT('',(1.5,0.,2.));
#4577=CARTESIAN_POINT('',(8.5,0.,2.));
#4578=CARTESIAN_POINT('Origin',(8.5,-3.,2.));
#4579=CARTESIAN_POINT('',(8.5,-3.,2.));
#4580=CARTESIAN_POINT('',(8.5,-3.,2.));
#4581=CARTESIAN_POINT('',(8.5,-3.,2.));
#4582=CARTESIAN_POINT('Origin',(1.5,-3.,2.));
#4583=CARTESIAN_POINT('',(1.5,-3.,2.));
#4584=CARTESIAN_POINT('',(1.5,-3.,2.));
#4585=CARTESIAN_POINT('',(1.5,-3.,2.));
#4586=CARTESIAN_POINT('Origin',(1.5,0.,2.));
#4587=CARTESIAN_POINT('',(1.5,0.,2.));
#4588=CARTESIAN_POINT('Origin',(5.,-1.5,2.));
#4589=CARTESIAN_POINT('',(0.,0.,0.));
#4590=CARTESIAN_POINT('Origin',(-0.1,0.82,-0.3));
#4591=CARTESIAN_POINT('',(0.,0.82,-0.3));
#4592=CARTESIAN_POINT('',(0.,1.,-0.3));
#4593=CARTESIAN_POINT('',(0.,0.41,-0.3));
#4594=CARTESIAN_POINT('',(10.,0.82,-0.3));
#4595=CARTESIAN_POINT('',(-0.1,0.82,-0.3));
#4596=CARTESIAN_POINT('',(10.,1.,-0.3));
#4597=CARTESIAN_POINT('',(10.,0.41,-0.3));
#4598=CARTESIAN_POINT('',(-0.05,1.,-0.3));
#4599=CARTESIAN_POINT('Origin',(-0.1,0.82,-0.55));
#4600=CARTESIAN_POINT('',(0.,0.82,-0.55));
#4601=CARTESIAN_POINT('',(0.,0.82,-0.275));
#4602=CARTESIAN_POINT('',(10.,0.82,-0.55));
#4603=CARTESIAN_POINT('',(-0.1,0.82,-0.55));
#4604=CARTESIAN_POINT('',(10.,0.82,-0.275));
#4605=CARTESIAN_POINT('Origin',(-0.1,0.67,-0.55));
#4606=CARTESIAN_POINT('',(0.,0.67,-0.55));
#4607=CARTESIAN_POINT('',(0.,0.335,-0.55));
#4608=CARTESIAN_POINT('',(10.,0.67,-0.55));
#4609=CARTESIAN_POINT('',(-0.1,0.67,-0.55));
#4610=CARTESIAN_POINT('',(10.,0.335,-0.55));
#4611=CARTESIAN_POINT('Origin',(-0.1,0.42,-0.3));
#4612=CARTESIAN_POINT('',(0.,0.42,-0.3));
#4613=CARTESIAN_POINT('',(0.,0.24,-0.12));
#4614=CARTESIAN_POINT('',(10.,0.42,-0.3));
#4615=CARTESIAN_POINT('',(-0.1,0.42,-0.3));
#4616=CARTESIAN_POINT('',(10.,0.24,-0.12));
#4617=CARTESIAN_POINT('Origin',(-0.1,0.42,0.3));
#4618=CARTESIAN_POINT('',(0.,0.42,0.3));
#4619=CARTESIAN_POINT('',(0.,0.42,0.15));
#4620=CARTESIAN_POINT('',(10.,0.42,0.3));
#4621=CARTESIAN_POINT('',(-0.1,0.42,0.3));
#4622=CARTESIAN_POINT('',(10.,0.42,0.15));
#4623=CARTESIAN_POINT('Origin',(-0.1,0.67,0.55));
#4624=CARTESIAN_POINT('',(0.,0.67,0.55));
#4625=CARTESIAN_POINT('',(6.93889390390723E-18,0.365,0.245));
#4626=CARTESIAN_POINT('',(10.,0.67,0.55));
#4627=CARTESIAN_POINT('',(-0.1,0.67,0.55));
#4628=CARTESIAN_POINT('',(10.,0.365,0.245));
#4629=CARTESIAN_POINT('Origin',(-0.1,0.82,0.55));
#4630=CARTESIAN_POINT('',(0.,0.82,0.55));
#4631=CARTESIAN_POINT('',(0.,0.41,0.55));
#4632=CARTESIAN_POINT('',(10.,0.82,0.55));
#4633=CARTESIAN_POINT('',(-0.1,0.82,0.55));
#4634=CARTESIAN_POINT('',(10.,0.41,0.55));
#4635=CARTESIAN_POINT('Origin',(-0.1,0.82,0.3));
#4636=CARTESIAN_POINT('',(0.,0.82,0.3));
#4637=CARTESIAN_POINT('',(0.,0.82,0.15));
#4638=CARTESIAN_POINT('',(10.,0.82,0.3));
#4639=CARTESIAN_POINT('',(-0.1,0.82,0.3));
#4640=CARTESIAN_POINT('',(10.,0.82,0.15));
#4641=CARTESIAN_POINT('Origin',(-0.1,1.05,0.3));
#4642=CARTESIAN_POINT('',(0.,1.,0.3));
#4643=CARTESIAN_POINT('',(0.,0.525,0.3));
#4644=CARTESIAN_POINT('',(10.,1.,0.3));
#4645=CARTESIAN_POINT('',(-0.05,1.,0.3));
#4646=CARTESIAN_POINT('',(10.,0.525,0.3));
#4647=CARTESIAN_POINT('Origin',(-0.1,-0.3,-0.82));
#4648=CARTESIAN_POINT('',(0.,-0.3,-0.82));
#4649=CARTESIAN_POINT('',(0.,-0.3,-1.));
#4650=CARTESIAN_POINT('',(0.,-0.3,-0.41));
#4651=CARTESIAN_POINT('',(10.,-0.3,-0.82));
#4652=CARTESIAN_POINT('',(-0.1,-0.3,-0.82));
#4653=CARTESIAN_POINT('',(10.,-0.3,-1.));
#4654=CARTESIAN_POINT('',(10.,-0.3,-0.41));
#4655=CARTESIAN_POINT('',(-0.05,-0.3,-1.));
#4656=CARTESIAN_POINT('Origin',(-0.1,-0.55,-0.82));
#4657=CARTESIAN_POINT('',(0.,-0.55,-0.82));
#4658=CARTESIAN_POINT('',(0.,-0.275,-0.82));
#4659=CARTESIAN_POINT('',(10.,-0.55,-0.82));
#4660=CARTESIAN_POINT('',(-0.1,-0.55,-0.82));
#4661=CARTESIAN_POINT('',(10.,-0.275,-0.82));
#4662=CARTESIAN_POINT('Origin',(-0.1,-0.55,-0.67));
#4663=CARTESIAN_POINT('',(0.,-0.55,-0.67));
#4664=CARTESIAN_POINT('',(0.,-0.55,-0.335));
#4665=CARTESIAN_POINT('',(10.,-0.55,-0.67));
#4666=CARTESIAN_POINT('',(-0.1,-0.55,-0.67));
#4667=CARTESIAN_POINT('',(10.,-0.55,-0.335));
#4668=CARTESIAN_POINT('Origin',(-0.1,-0.3,-0.42));
#4669=CARTESIAN_POINT('',(0.,-0.3,-0.42));
#4670=CARTESIAN_POINT('',(0.,-0.12,-0.24));
#4671=CARTESIAN_POINT('',(10.,-0.3,-0.42));
#4672=CARTESIAN_POINT('',(-0.1,-0.3,-0.42));
#4673=CARTESIAN_POINT('',(10.,-0.12,-0.24));
#4674=CARTESIAN_POINT('Origin',(-0.1,0.3,-0.42));
#4675=CARTESIAN_POINT('',(0.,0.3,-0.42));
#4676=CARTESIAN_POINT('',(0.,0.15,-0.42));
#4677=CARTESIAN_POINT('',(10.,0.3,-0.42));
#4678=CARTESIAN_POINT('',(-0.1,0.3,-0.42));
#4679=CARTESIAN_POINT('',(10.,0.15,-0.42));
#4680=CARTESIAN_POINT('Origin',(-0.1,0.55,-0.67));
#4681=CARTESIAN_POINT('',(0.,0.55,-0.67));
#4682=CARTESIAN_POINT('',(0.,0.245,-0.365));
#4683=CARTESIAN_POINT('',(10.,0.55,-0.67));
#4684=CARTESIAN_POINT('',(-0.1,0.55,-0.67));
#4685=CARTESIAN_POINT('',(10.,0.245,-0.365));
#4686=CARTESIAN_POINT('Origin',(-0.1,0.55,-0.82));
#4687=CARTESIAN_POINT('',(0.,0.55,-0.82));
#4688=CARTESIAN_POINT('',(0.,0.55,-0.41));
#4689=CARTESIAN_POINT('',(10.,0.55,-0.82));
#4690=CARTESIAN_POINT('',(-0.1,0.55,-0.82));
#4691=CARTESIAN_POINT('',(10.,0.55,-0.41));
#4692=CARTESIAN_POINT('Origin',(-0.1,0.3,-0.82));
#4693=CARTESIAN_POINT('',(0.,0.3,-0.82));
#4694=CARTESIAN_POINT('',(0.,0.15,-0.82));
#4695=CARTESIAN_POINT('',(10.,0.3,-0.82));
#4696=CARTESIAN_POINT('',(-0.1,0.3,-0.82));
#4697=CARTESIAN_POINT('',(10.,0.15,-0.82));
#4698=CARTESIAN_POINT('Origin',(-0.1,0.3,-1.05));
#4699=CARTESIAN_POINT('',(0.,0.3,-1.));
#4700=CARTESIAN_POINT('',(0.,0.3,-0.525));
#4701=CARTESIAN_POINT('',(10.,0.3,-1.));
#4702=CARTESIAN_POINT('',(-0.05,0.3,-1.));
#4703=CARTESIAN_POINT('',(10.,0.3,-0.525));
#4704=CARTESIAN_POINT('Origin',(-0.1,-0.82,0.3));
#4705=CARTESIAN_POINT('',(0.,-0.82,0.3));
#4706=CARTESIAN_POINT('',(0.,-1.,0.3));
#4707=CARTESIAN_POINT('',(0.,-0.41,0.3));
#4708=CARTESIAN_POINT('',(10.,-0.82,0.3));
#4709=CARTESIAN_POINT('',(-0.1,-0.82,0.3));
#4710=CARTESIAN_POINT('',(10.,-1.,0.3));
#4711=CARTESIAN_POINT('',(10.,-0.41,0.3));
#4712=CARTESIAN_POINT('',(-0.05,-1.,0.3));
#4713=CARTESIAN_POINT('Origin',(-0.1,-0.82,0.55));
#4714=CARTESIAN_POINT('',(0.,-0.82,0.55));
#4715=CARTESIAN_POINT('',(0.,-0.82,0.275));
#4716=CARTESIAN_POINT('',(10.,-0.82,0.55));
#4717=CARTESIAN_POINT('',(-0.1,-0.82,0.55));
#4718=CARTESIAN_POINT('',(10.,-0.82,0.275));
#4719=CARTESIAN_POINT('Origin',(-0.1,-0.67,0.55));
#4720=CARTESIAN_POINT('',(0.,-0.67,0.55));
#4721=CARTESIAN_POINT('',(0.,-0.335,0.55));
#4722=CARTESIAN_POINT('',(10.,-0.67,0.55));
#4723=CARTESIAN_POINT('',(-0.1,-0.67,0.55));
#4724=CARTESIAN_POINT('',(10.,-0.335,0.55));
#4725=CARTESIAN_POINT('Origin',(-0.1,-0.42,0.3));
#4726=CARTESIAN_POINT('',(0.,-0.42,0.3));
#4727=CARTESIAN_POINT('',(-6.93889390390723E-18,-0.24,0.12));
#4728=CARTESIAN_POINT('',(10.,-0.42,0.3));
#4729=CARTESIAN_POINT('',(-0.1,-0.42,0.3));
#4730=CARTESIAN_POINT('',(10.,-0.24,0.12));
#4731=CARTESIAN_POINT('Origin',(-0.1,-0.42,-0.3));
#4732=CARTESIAN_POINT('',(0.,-0.42,-0.3));
#4733=CARTESIAN_POINT('',(0.,-0.42,-0.15));
#4734=CARTESIAN_POINT('',(10.,-0.42,-0.3));
#4735=CARTESIAN_POINT('',(-0.1,-0.42,-0.3));
#4736=CARTESIAN_POINT('',(10.,-0.42,-0.15));
#4737=CARTESIAN_POINT('Origin',(-0.1,-0.67,-0.55));
#4738=CARTESIAN_POINT('',(0.,-0.67,-0.55));
#4739=CARTESIAN_POINT('',(0.,-0.365,-0.245));
#4740=CARTESIAN_POINT('',(10.,-0.67,-0.55));
#4741=CARTESIAN_POINT('',(-0.1,-0.67,-0.55));
#4742=CARTESIAN_POINT('',(10.,-0.365,-0.245));
#4743=CARTESIAN_POINT('Origin',(-0.1,-0.82,-0.55));
#4744=CARTESIAN_POINT('',(0.,-0.82,-0.55));
#4745=CARTESIAN_POINT('',(0.,-0.41,-0.55));
#4746=CARTESIAN_POINT('',(10.,-0.82,-0.55));
#4747=CARTESIAN_POINT('',(-0.1,-0.82,-0.55));
#4748=CARTESIAN_POINT('',(10.,-0.41,-0.55));
#4749=CARTESIAN_POINT('Origin',(-0.1,-0.82,-0.3));
#4750=CARTESIAN_POINT('',(0.,-0.82,-0.3));
#4751=CARTESIAN_POINT('',(0.,-0.82,-0.15));
#4752=CARTESIAN_POINT('',(10.,-0.82,-0.3));
#4753=CARTESIAN_POINT('',(-0.1,-0.82,-0.3));
#4754=CARTESIAN_POINT('',(10.,-0.82,-0.15));
#4755=CARTESIAN_POINT('Origin',(-0.1,-1.05,-0.3));
#4756=CARTESIAN_POINT('',(0.,-1.,-0.3));
#4757=CARTESIAN_POINT('',(0.,-0.525,-0.3));
#4758=CARTESIAN_POINT('',(10.,-1.,-0.3));
#4759=CARTESIAN_POINT('',(-0.05,-1.,-0.3));
#4760=CARTESIAN_POINT('',(10.,-0.525,-0.3));
#4761=CARTESIAN_POINT('Origin',(-0.1,0.3,0.82));
#4762=CARTESIAN_POINT('',(0.,0.3,0.82));
#4763=CARTESIAN_POINT('',(0.,0.3,1.));
#4764=CARTESIAN_POINT('',(0.,0.3,0.41));
#4765=CARTESIAN_POINT('',(10.,0.3,0.82));
#4766=CARTESIAN_POINT('',(-0.1,0.3,0.82));
#4767=CARTESIAN_POINT('',(10.,0.3,1.));
#4768=CARTESIAN_POINT('',(10.,0.3,0.41));
#4769=CARTESIAN_POINT('',(-0.05,0.3,1.));
#4770=CARTESIAN_POINT('Origin',(-0.1,0.55,0.82));
#4771=CARTESIAN_POINT('',(0.,0.55,0.82));
#4772=CARTESIAN_POINT('',(0.,0.275,0.82));
#4773=CARTESIAN_POINT('',(10.,0.55,0.82));
#4774=CARTESIAN_POINT('',(-0.1,0.55,0.82));
#4775=CARTESIAN_POINT('',(10.,0.275,0.82));
#4776=CARTESIAN_POINT('Origin',(-0.1,0.55,0.67));
#4777=CARTESIAN_POINT('',(0.,0.55,0.67));
#4778=CARTESIAN_POINT('',(0.,0.55,0.335));
#4779=CARTESIAN_POINT('',(10.,0.55,0.67));
#4780=CARTESIAN_POINT('',(-0.1,0.55,0.67));
#4781=CARTESIAN_POINT('',(10.,0.55,0.335));
#4782=CARTESIAN_POINT('Origin',(-0.1,0.3,0.42));
#4783=CARTESIAN_POINT('',(0.,0.3,0.42));
#4784=CARTESIAN_POINT('',(6.93889390390723E-18,0.12,0.24));
#4785=CARTESIAN_POINT('',(10.,0.3,0.42));
#4786=CARTESIAN_POINT('',(-0.1,0.3,0.42));
#4787=CARTESIAN_POINT('',(10.,0.12,0.24));
#4788=CARTESIAN_POINT('Origin',(-0.1,-0.3,0.42));
#4789=CARTESIAN_POINT('',(0.,-0.3,0.42));
#4790=CARTESIAN_POINT('',(0.,-0.15,0.42));
#4791=CARTESIAN_POINT('',(10.,-0.3,0.42));
#4792=CARTESIAN_POINT('',(-0.1,-0.3,0.42));
#4793=CARTESIAN_POINT('',(10.,-0.15,0.42));
#4794=CARTESIAN_POINT('Origin',(-0.1,-0.55,0.67));
#4795=CARTESIAN_POINT('',(0.,-0.55,0.67));
#4796=CARTESIAN_POINT('',(6.93889390390723E-18,-0.245,0.365));
#4797=CARTESIAN_POINT('',(10.,-0.55,0.67));
#4798=CARTESIAN_POINT('',(-0.1,-0.55,0.67));
#4799=CARTESIAN_POINT('',(10.,-0.245,0.365));
#4800=CARTESIAN_POINT('Origin',(-0.1,-0.55,0.82));
#4801=CARTESIAN_POINT('',(0.,-0.55,0.82));
#4802=CARTESIAN_POINT('',(0.,-0.55,0.41));
#4803=CARTESIAN_POINT('',(10.,-0.55,0.82));
#4804=CARTESIAN_POINT('',(-0.1,-0.55,0.82));
#4805=CARTESIAN_POINT('',(10.,-0.55,0.41));
#4806=CARTESIAN_POINT('Origin',(-0.1,-0.3,0.82));
#4807=CARTESIAN_POINT('',(0.,-0.3,0.82));
#4808=CARTESIAN_POINT('',(0.,-0.15,0.82));
#4809=CARTESIAN_POINT('',(10.,-0.3,0.82));
#4810=CARTESIAN_POINT('',(-0.1,-0.3,0.82));
#4811=CARTESIAN_POINT('',(10.,-0.15,0.82));
#4812=CARTESIAN_POINT('Origin',(-0.1,-0.3,1.05));
#4813=CARTESIAN_POINT('',(0.,-0.3,1.));
#4814=CARTESIAN_POINT('',(0.,-0.3,0.525));
#4815=CARTESIAN_POINT('',(10.,-0.3,1.));
#4816=CARTESIAN_POINT('',(-0.05,-0.3,1.));
#4817=CARTESIAN_POINT('',(10.,-0.3,0.525));
#4818=CARTESIAN_POINT('Origin',(-0.1,0.,0.));
#4819=CARTESIAN_POINT('',(0.,-2.57175827820944E-17,0.21));
#4820=CARTESIAN_POINT('Origin',(0.,0.,0.));
#4821=CARTESIAN_POINT('',(10.,2.57175827820944E-17,0.21));
#4822=CARTESIAN_POINT('',(-0.1,-2.57175827820944E-17,0.21));
#4823=CARTESIAN_POINT('Origin',(10.,0.,0.));
#4824=CARTESIAN_POINT('Origin',(0.,1.,-1.));
#4825=CARTESIAN_POINT('',(0.,1.,1.));
#4826=CARTESIAN_POINT('',(0.,1.,-1.));
#4827=CARTESIAN_POINT('',(10.,1.,1.));
#4828=CARTESIAN_POINT('',(0.,1.,1.));
#4829=CARTESIAN_POINT('',(10.,1.,-1.));
#4830=CARTESIAN_POINT('Origin',(0.,1.,-1.));
#4831=CARTESIAN_POINT('',(10.,1.,-1.));
#4832=CARTESIAN_POINT('',(10.,1.,-1.));
#4833=CARTESIAN_POINT('',(0.,1.,-1.));
#4834=CARTESIAN_POINT('',(0.,1.,-1.));
#4835=CARTESIAN_POINT('',(0.,1.,-1.));
#4836=CARTESIAN_POINT('Origin',(0.,-1.,-1.));
#4837=CARTESIAN_POINT('',(0.,-1.,-1.));
#4838=CARTESIAN_POINT('',(10.,-1.,-1.));
#4839=CARTESIAN_POINT('Origin',(0.,-1.,-1.));
#4840=CARTESIAN_POINT('',(10.,-1.,-1.));
#4841=CARTESIAN_POINT('',(10.,-1.,-1.));
#4842=CARTESIAN_POINT('',(0.,-1.,-1.));
#4843=CARTESIAN_POINT('',(0.,-1.,-1.));
#4844=CARTESIAN_POINT('',(0.,-1.,-1.));
#4845=CARTESIAN_POINT('Origin',(0.,-1.,1.));
#4846=CARTESIAN_POINT('',(0.,-1.,1.));
#4847=CARTESIAN_POINT('',(10.,-1.,1.));
#4848=CARTESIAN_POINT('Origin',(0.,-1.,1.));
#4849=CARTESIAN_POINT('',(10.,-1.,1.));
#4850=CARTESIAN_POINT('',(10.,-1.,1.));
#4851=CARTESIAN_POINT('',(0.,-1.,1.));
#4852=CARTESIAN_POINT('',(0.,-1.,1.));
#4853=CARTESIAN_POINT('',(0.,-1.,1.));
#4854=CARTESIAN_POINT('Origin',(0.,1.,1.));
#4855=CARTESIAN_POINT('',(0.,1.,1.));
#4856=CARTESIAN_POINT('',(10.,1.,1.));
#4857=CARTESIAN_POINT('Origin',(0.,1.,1.));
#4858=CARTESIAN_POINT('',(10.,1.,1.));
#4859=CARTESIAN_POINT('',(0.,1.,1.));
#4860=CARTESIAN_POINT('Origin',(10.,0.,0.));
#4861=CARTESIAN_POINT('Origin',(0.,0.,0.));
#4862=CARTESIAN_POINT('',(0.,0.,0.));
#4863=CARTESIAN_POINT('Origin',(0.,0.395,0.25));
#4864=CARTESIAN_POINT('',(-0.5,0.3,0.25));
#4865=CARTESIAN_POINT('',(0.5,0.3,0.25));
#4866=CARTESIAN_POINT('',(0.25,0.3,0.25));
#4867=CARTESIAN_POINT('',(-0.5,0.5,0.25));
#4868=CARTESIAN_POINT('',(-0.5,0.5,0.25));
#4869=CARTESIAN_POINT('',(0.5,0.5,0.25));
#4870=CARTESIAN_POINT('',(0.5,0.5,0.25));
#4871=CARTESIAN_POINT('',(0.5,0.29,0.25));
#4872=CARTESIAN_POINT('Origin',(0.5,0.5,0.25));
#4873=CARTESIAN_POINT('',(-0.5,0.5,0.4));
#4874=CARTESIAN_POINT('',(-0.5,0.5,0.25));
#4875=CARTESIAN_POINT('',(0.5,0.5,0.4));
#4876=CARTESIAN_POINT('',(0.5,0.5,0.4));
#4877=CARTESIAN_POINT('',(0.5,0.5,0.25));
#4878=CARTESIAN_POINT('Origin',(0.,0.,0.4));
#4879=CARTESIAN_POINT('',(-0.5,-0.5,0.4));
#4880=CARTESIAN_POINT('',(-0.5,0.5,0.4));
#4881=CARTESIAN_POINT('',(0.5,-0.5,0.4));
#4882=CARTESIAN_POINT('',(-0.5,-0.5,0.4));
#4883=CARTESIAN_POINT('',(0.5,-0.3,0.4));
#4884=CARTESIAN_POINT('',(-0.2117,2.59257727379495E-17,0.4));
#4885=CARTESIAN_POINT('Origin',(0.,0.,0.4));
#4886=CARTESIAN_POINT('Origin',(-0.5,0.3,0.));
#4887=CARTESIAN_POINT('',(-0.5,0.3,0.15));
#4888=CARTESIAN_POINT('',(-0.5,0.3,0.));
#4889=CARTESIAN_POINT('',(-0.5,0.15,0.));
#4890=CARTESIAN_POINT('',(-0.5,0.225,0.075));
#4891=CARTESIAN_POINT('',(-0.5,-0.15,0.));
#4892=CARTESIAN_POINT('',(-0.5,0.3,0.));
#4893=CARTESIAN_POINT('',(-0.5,-0.3,0.15));
#4894=CARTESIAN_POINT('',(-0.5,-0.075,-0.075));
#4895=CARTESIAN_POINT('',(-0.5,-0.3,0.25));
#4896=CARTESIAN_POINT('',(-0.5,-0.3,0.));
#4897=CARTESIAN_POINT('',(-0.5,-0.5,0.25));
#4898=CARTESIAN_POINT('',(-0.5,-0.29,0.25));
#4899=CARTESIAN_POINT('',(-0.5,-0.5,0.25));
#4900=CARTESIAN_POINT('Origin',(-0.5,-0.5,0.25));
#4901=CARTESIAN_POINT('',(0.5,-0.5,0.25));
#4902=CARTESIAN_POINT('',(-0.5,-0.5,0.25));
#4903=CARTESIAN_POINT('',(0.5,-0.5,0.25));
#4904=CARTESIAN_POINT('Origin',(0.,-0.395,0.25));
#4905=CARTESIAN_POINT('',(0.5,-0.3,0.25));
#4906=CARTESIAN_POINT('',(-0.25,-0.3,0.25));
#4907=CARTESIAN_POINT('',(0.5,-0.5,0.25));
#4908=CARTESIAN_POINT('Origin',(0.5,-0.3,0.));
#4909=CARTESIAN_POINT('',(0.5,-0.3,0.15));
#4910=CARTESIAN_POINT('',(0.5,-0.3,0.));
#4911=CARTESIAN_POINT('',(0.5,-0.15,0.));
#4912=CARTESIAN_POINT('',(0.5,-0.225,0.075));
#4913=CARTESIAN_POINT('',(0.5,0.15,0.));
#4914=CARTESIAN_POINT('',(0.5,-0.3,0.));
#4915=CARTESIAN_POINT('',(0.5,0.3,0.15));
#4916=CARTESIAN_POINT('',(0.5,0.075,-0.075));
#4917=CARTESIAN_POINT('',(0.5,0.3,0.));
#4918=CARTESIAN_POINT('Origin',(-0.5,-0.3,0.));
#4919=CARTESIAN_POINT('',(-0.25,-0.3,0.15));
#4920=CARTESIAN_POINT('Origin',(-0.25,-0.225,0.075));
#4921=CARTESIAN_POINT('',(-0.149388386429468,-0.15,0.));
#4922=CARTESIAN_POINT('',(-0.25,-0.15,0.));
#4923=CARTESIAN_POINT('',(0.149388386429468,-0.15,0.));
#4924=CARTESIAN_POINT('Origin',(0.,0.,-0.15));
#4925=CARTESIAN_POINT('',(-0.25,-0.15,0.));
#4926=CARTESIAN_POINT('Origin',(0.,0.,-0.1));
#4927=CARTESIAN_POINT('',(-0.2117,-2.59257727379495E-17,0.));
#4928=CARTESIAN_POINT('Origin',(0.,0.,0.));
#4929=CARTESIAN_POINT('',(-0.2117,-2.59257727379495E-17,-0.1));
#4930=CARTESIAN_POINT('',(-0.149388386429468,0.15,0.));
#4931=CARTESIAN_POINT('Origin',(0.,0.,0.));
#4932=CARTESIAN_POINT('',(0.149388386429468,0.15,0.));
#4933=CARTESIAN_POINT('Origin',(0.,0.,-0.15));
#4934=CARTESIAN_POINT('Origin',(0.,0.,0.));
#4935=CARTESIAN_POINT('Origin',(0.,0.,0.));
#4936=CARTESIAN_POINT('',(0.25,0.15,0.));
#4937=CARTESIAN_POINT('Origin',(0.,0.,0.));
#4938=CARTESIAN_POINT('',(0.25,0.15,0.));
#4939=CARTESIAN_POINT('Origin',(0.25,0.225,0.075));
#4940=CARTESIAN_POINT('',(0.25,0.3,0.15));
#4941=CARTESIAN_POINT('Origin',(0.5,0.3,0.));
#4942=CARTESIAN_POINT('',(0.,0.,0.));
#4943=CARTESIAN_POINT('Origin',(0.,0.09,0.));
#4944=CARTESIAN_POINT('',(-0.285,0.1,3.49024337756996E-17));
#4945=CARTESIAN_POINT('Origin',(0.,0.1,0.));
#4946=CARTESIAN_POINT('',(-0.265,0.08,-3.24531401774049E-17));
#4947=CARTESIAN_POINT('',(-0.275,0.09,3.36777869765522E-17));
#4948=CARTESIAN_POINT('Origin',(0.,0.08,0.));
#4949=CARTESIAN_POINT('Origin',(0.,0.,0.));
#4950=CARTESIAN_POINT('',(-0.265,0.,3.24531401774049E-17));
#4951=CARTESIAN_POINT('',(-0.265,0.,3.24531401774049E-17));
#4952=CARTESIAN_POINT('Origin',(0.,0.,0.));
#4953=CARTESIAN_POINT('Origin',(0.,0.1,0.));
#4954=CARTESIAN_POINT('',(-0.5,0.1,6.12323399573677E-17));
#4955=CARTESIAN_POINT('Origin',(0.,0.1,0.));
#4956=CARTESIAN_POINT('Origin',(0.,0.,0.));
#4957=CARTESIAN_POINT('',(-0.5,0.,6.12323399573677E-17));
#4958=CARTESIAN_POINT('',(-0.5,0.,6.12323399573677E-17));
#4959=CARTESIAN_POINT('Origin',(0.,0.,0.));
#4960=CARTESIAN_POINT('Origin',(0.,0.,0.));
#4961=CARTESIAN_POINT('',(0.,0.,0.));
#4962=CARTESIAN_POINT('Origin',(0.115470053837925,-0.5,-0.2));
#4963=CARTESIAN_POINT('',(0.23094010767585,-0.5,0.));
#4964=CARTESIAN_POINT('',(0.115470053837925,-0.5,-0.2));
#4965=CARTESIAN_POINT('',(0.23094010767585,-0.5,0.));
#4966=CARTESIAN_POINT('',(0.115470053837925,-0.8,-0.2));
#4967=CARTESIAN_POINT('',(0.115470053837925,-0.5,-0.2));
#4968=CARTESIAN_POINT('',(0.23094010767585,-0.8,0.));
#4969=CARTESIAN_POINT('',(0.23094010767585,-0.8,0.));
#4970=CARTESIAN_POINT('',(0.23094010767585,-0.5,0.));
#4971=CARTESIAN_POINT('Origin',(-0.115470053837925,-0.5,-0.2));
#4972=CARTESIAN_POINT('',(-0.115470053837925,-0.5,-0.2));
#4973=CARTESIAN_POINT('',(0.115470053837925,-0.5,-0.2));
#4974=CARTESIAN_POINT('',(-0.115470053837925,-0.8,-0.2));
#4975=CARTESIAN_POINT('',(-0.115470053837925,-0.5,-0.2));
#4976=CARTESIAN_POINT('',(0.115470053837925,-0.8,-0.2));
#4977=CARTESIAN_POINT('Origin',(-0.23094010767585,-0.5,-2.77555756156289E-17));
#4978=CARTESIAN_POINT('',(-0.23094010767585,-0.5,-2.82820063659975E-17));
#4979=CARTESIAN_POINT('',(-0.115470053837925,-0.5,-0.2));
#4980=CARTESIAN_POINT('',(-0.23094010767585,-0.8,-2.77555756156289E-17));
#4981=CARTESIAN_POINT('',(-0.23094010767585,-0.5,-2.82820063659975E-17));
#4982=CARTESIAN_POINT('',(-0.115470053837925,-0.8,-0.2));
#4983=CARTESIAN_POINT('Origin',(-0.115470053837925,-0.5,0.2));
#4984=CARTESIAN_POINT('',(-0.115470053837925,-0.5,0.2));
#4985=CARTESIAN_POINT('',(-0.23094010767585,-0.5,-2.82820063659975E-17));
#4986=CARTESIAN_POINT('',(-0.115470053837925,-0.8,0.2));
#4987=CARTESIAN_POINT('',(-0.115470053837925,-0.5,0.2));
#4988=CARTESIAN_POINT('',(-0.23094010767585,-0.8,-2.82820063659975E-17));
#4989=CARTESIAN_POINT('Origin',(0.115470053837925,-0.5,0.2));
#4990=CARTESIAN_POINT('',(0.115470053837925,-0.5,0.2));
#4991=CARTESIAN_POINT('',(-0.115470053837925,-0.5,0.2));
#4992=CARTESIAN_POINT('',(0.115470053837925,-0.8,0.2));
#4993=CARTESIAN_POINT('',(0.115470053837925,-0.5,0.2));
#4994=CARTESIAN_POINT('',(-0.115470053837925,-0.8,0.2));
#4995=CARTESIAN_POINT('Origin',(0.23094010767585,-0.5,0.));
#4996=CARTESIAN_POINT('',(0.115470053837925,-0.5,0.2));
#4997=CARTESIAN_POINT('',(0.115470053837925,-0.8,0.2));
#4998=CARTESIAN_POINT('Origin',(0.,-0.5,0.));
#4999=CARTESIAN_POINT('Origin',(0.,-0.8,0.));
#5000=CARTESIAN_POINT('Origin',(0.,-1.4,0.));
#5001=CARTESIAN_POINT('',(-0.24505,-1.4,3.00099698131059E-17));
#5002=CARTESIAN_POINT('Origin',(0.,-1.4,0.));
#5003=CARTESIAN_POINT('Origin',(0.375,0.5,0.));
#5004=CARTESIAN_POINT('',(-0.375,0.5,-4.59242549680257E-17));
#5005=CARTESIAN_POINT('Origin',(0.,0.5,0.));
#5006=CARTESIAN_POINT('Origin',(0.,0.475,0.));
#5007=CARTESIAN_POINT('',(-0.425,0.45,-5.20474889637625E-17));
#5008=CARTESIAN_POINT('Origin',(0.,0.45,0.));
#5009=CARTESIAN_POINT('',(-0.4,0.475,-4.89858719658941E-17));
#5010=CARTESIAN_POINT('Origin',(0.,0.24,0.));
#5011=CARTESIAN_POINT('',(-0.425,0.0299999999999998,-5.20474889637625E-17));
#5012=CARTESIAN_POINT('Origin',(0.,0.0299999999999998,0.));
#5013=CARTESIAN_POINT('',(-0.425,0.24,-5.20474889637625E-17));
#5014=CARTESIAN_POINT('Origin',(0.,0.0150000000000001,0.));
#5015=CARTESIAN_POINT('',(-0.395,4.85722573273506E-17,-4.83735485663204E-17));
#5016=CARTESIAN_POINT('Origin',(0.,0.,0.));
#5017=CARTESIAN_POINT('',(-0.41,0.0150000000000001,-5.02105187650415E-17));
#5018=CARTESIAN_POINT('Origin',(0.27,0.,0.));
#5019=CARTESIAN_POINT('',(-0.27,0.,-3.30654635769785E-17));
#5020=CARTESIAN_POINT('Origin',(0.,0.,0.));
#5021=CARTESIAN_POINT('Origin',(0.,-0.02,0.));
#5022=CARTESIAN_POINT('',(-0.24505,-0.0498999999999999,3.00099698131059E-17));
#5023=CARTESIAN_POINT('Origin',(0.,-0.0498999999999999,0.));
#5024=CARTESIAN_POINT('',(-0.26,-0.02,-3.18408167778312E-17));
#5025=CARTESIAN_POINT('Origin',(0.,-0.995,0.));
#5026=CARTESIAN_POINT('',(-0.24505,-0.995,-3.00099698131059E-17));
#5027=CARTESIAN_POINT('',(0.,0.,0.));
#5028=CARTESIAN_POINT('',(0.,0.,0.));
#5029=CARTESIAN_POINT('',(0.,0.,0.));
#5030=CARTESIAN_POINT('Origin',(5.,0.06,8.));
#5031=CARTESIAN_POINT('',(4.575,0.16,8.));
#5032=CARTESIAN_POINT('Origin',(5.,0.16,8.));
#5033=CARTESIAN_POINT('',(4.575,0.96,8.));
#5034=CARTESIAN_POINT('',(4.575,0.06,8.));
#5035=CARTESIAN_POINT('Origin',(5.,0.96,8.));
#5036=CARTESIAN_POINT('Origin',(15.,0.06,8.));
#5037=CARTESIAN_POINT('',(14.575,0.16,8.));
#5038=CARTESIAN_POINT('Origin',(15.,0.16,8.));
#5039=CARTESIAN_POINT('',(14.575,0.96,8.));
#5040=CARTESIAN_POINT('',(14.575,0.06,8.));
#5041=CARTESIAN_POINT('Origin',(15.,0.96,8.));
#5042=CARTESIAN_POINT('Origin',(15.,0.16,8.));
#5043=CARTESIAN_POINT('',(13.8819660112501,0.96,7.));
#5044=CARTESIAN_POINT('',(13.8819660112501,0.16,7.));
#5045=CARTESIAN_POINT('',(13.8819660112501,0.16,7.));
#5046=CARTESIAN_POINT('',(13.8819660112501,0.96,9.));
#5047=CARTESIAN_POINT('Origin',(15.,0.96,8.));
#5048=CARTESIAN_POINT('',(13.8819660112501,0.16,9.));
#5049=CARTESIAN_POINT('',(13.8819660112501,0.16,9.));
#5050=CARTESIAN_POINT('Origin',(15.,0.16,8.));
#5051=CARTESIAN_POINT('Origin',(15.,0.16,7.));
#5052=CARTESIAN_POINT('',(6.11803398874989,0.16,7.));
#5053=CARTESIAN_POINT('',(5.,0.16,7.));
#5054=CARTESIAN_POINT('',(6.11803398874989,0.96,7.));
#5055=CARTESIAN_POINT('',(6.11803398874989,0.16,7.));
#5056=CARTESIAN_POINT('',(5.,0.96,7.));
#5057=CARTESIAN_POINT('Origin',(5.,0.16,8.));
#5058=CARTESIAN_POINT('',(6.11803398874989,0.16,9.));
#5059=CARTESIAN_POINT('',(15.,0.16,9.));
#5060=CARTESIAN_POINT('Origin',(5.,0.16,8.));
#5061=CARTESIAN_POINT('Origin',(5.,0.16,9.));
#5062=CARTESIAN_POINT('',(6.11803398874989,0.96,9.));
#5063=CARTESIAN_POINT('',(15.,0.96,9.));
#5064=CARTESIAN_POINT('',(6.11803398874989,0.16,9.));
#5065=CARTESIAN_POINT('Origin',(5.,0.16,8.));
#5066=CARTESIAN_POINT('Origin',(5.,0.96,8.));
#5067=CARTESIAN_POINT('Origin',(5.,0.96,8.));
#5068=CARTESIAN_POINT('',(0.,0.,0.));
#5069=CARTESIAN_POINT('Origin',(0.,-1.935,0.));
#5070=CARTESIAN_POINT('',(-0.3933,-3.9267,4.81653586104654E-17));
#5071=CARTESIAN_POINT('Origin',(0.,-3.9267,0.));
#5072=CARTESIAN_POINT('',(-0.3933,0.,-4.81653586104654E-17));
#5073=CARTESIAN_POINT('',(-0.3933,-1.935,-4.81653586104654E-17));
#5074=CARTESIAN_POINT('Origin',(0.,0.,0.));
#5075=CARTESIAN_POINT('Origin',(0.,-3.96,0.));
#5076=CARTESIAN_POINT('',(-0.32,-4.,-3.91886975727153E-17));
#5077=CARTESIAN_POINT('Origin',(0.,-4.,0.));
#5078=CARTESIAN_POINT('',(-0.36,-3.96,-4.40872847693047E-17));
#5079=CARTESIAN_POINT('Origin',(0.,-4.,0.));
#5080=CARTESIAN_POINT('Origin',(0.,0.462722715486149,0.));
#5081=CARTESIAN_POINT('',(-0.6175,0.53,-7.5621939847349E-17));
#5082=CARTESIAN_POINT('Origin',(0.,0.53,0.));
#5083=CARTESIAN_POINT('',(-0.750555349946514,0.453180457891261,-9.19165206894919E-17));
#5084=CARTESIAN_POINT('',(-0.734027674973257,0.462722715486149,-8.98924642641573E-17));
#5085=CARTESIAN_POINT('',(-0.375277674973257,0.453180457891261,0.65));
#5086=CARTESIAN_POINT('Ctrl Pts',(-0.375277674973257,0.45318045789126,0.65));
#5087=CARTESIAN_POINT('Ctrl Pts',(-0.562916512459968,0.561513791224244,
0.324999999999856));
#5088=CARTESIAN_POINT('Ctrl Pts',(-0.750555349946514,0.45318045789126,-9.19165206894919E-17));
#5089=CARTESIAN_POINT('',(0.375277674973257,0.453180457891261,0.65));
#5090=CARTESIAN_POINT('Ctrl Pts',(0.375277674973257,0.453180457891261,0.65));
#5091=CARTESIAN_POINT('Ctrl Pts',(-1.66922031752392E-13,0.561513791224244,
0.65));
#5092=CARTESIAN_POINT('Ctrl Pts',(-0.375277674973257,0.45318045789126,0.65));
#5093=CARTESIAN_POINT('',(0.750555349946514,0.453180457891261,0.));
#5094=CARTESIAN_POINT('Ctrl Pts',(0.750555349946514,0.453180457891261,0.));
#5095=CARTESIAN_POINT('Ctrl Pts',(0.562916512459802,0.561513791224244,0.325000000000144));
#5096=CARTESIAN_POINT('Ctrl Pts',(0.375277674973257,0.45318045789126,0.65));
#5097=CARTESIAN_POINT('',(0.375277674973257,0.453180457891261,-0.65));
#5098=CARTESIAN_POINT('Ctrl Pts',(0.375277674973257,0.45318045789126,-0.65));
#5099=CARTESIAN_POINT('Ctrl Pts',(0.562916512459968,0.561513791224244,-0.324999999999855));
#5100=CARTESIAN_POINT('Ctrl Pts',(0.750555349946514,0.453180457891261,0.));
#5101=CARTESIAN_POINT('',(-0.375277674973257,0.45318045789126,-0.65));
#5102=CARTESIAN_POINT('Ctrl Pts',(-0.375277674973257,0.453180457891261,
-0.65));
#5103=CARTESIAN_POINT('Ctrl Pts',(1.66866520601161E-13,0.561513791224244,
-0.65));
#5104=CARTESIAN_POINT('Ctrl Pts',(0.375277674973257,0.45318045789126,-0.65));
#5105=CARTESIAN_POINT('Ctrl Pts',(-0.750555349946514,0.453180457891261,
-9.19165206894919E-17));
#5106=CARTESIAN_POINT('Ctrl Pts',(-0.562916512459802,0.561513791224244,
-0.325000000000144));
#5107=CARTESIAN_POINT('Ctrl Pts',(-0.375277674973257,0.45318045789126,-0.65));
#5108=CARTESIAN_POINT('Origin',(0.375277674973257,0.,-0.65));
#5109=CARTESIAN_POINT('',(0.375277674973257,0.,-0.65));
#5110=CARTESIAN_POINT('',(0.375277674973257,0.,-0.65));
#5111=CARTESIAN_POINT('',(-0.375277674973257,0.,-0.65));
#5112=CARTESIAN_POINT('',(0.375277674973257,0.,-0.65));
#5113=CARTESIAN_POINT('',(-0.375277674973257,0.,-0.65));
#5114=CARTESIAN_POINT('Origin',(0.750555349946514,0.,0.));
#5115=CARTESIAN_POINT('',(0.750555349946514,0.,0.));
#5116=CARTESIAN_POINT('',(0.750555349946514,0.,0.));
#5117=CARTESIAN_POINT('',(0.750555349946514,0.,0.));
#5118=CARTESIAN_POINT('Origin',(0.375277674973257,0.,0.65));
#5119=CARTESIAN_POINT('',(0.375277674973257,0.,0.65));
#5120=CARTESIAN_POINT('',(0.375277674973257,0.,0.65));
#5121=CARTESIAN_POINT('',(0.375277674973257,0.,0.65));
#5122=CARTESIAN_POINT('Origin',(-0.375277674973257,0.,0.65));
#5123=CARTESIAN_POINT('',(-0.375277674973257,0.,0.65));
#5124=CARTESIAN_POINT('',(-0.375277674973257,0.,0.65));
#5125=CARTESIAN_POINT('',(-0.375277674973257,0.,0.65));
#5126=CARTESIAN_POINT('Origin',(-0.750555349946514,0.,-9.19165206894919E-17));
#5127=CARTESIAN_POINT('',(-0.750555349946514,0.,-9.19165206894919E-17));
#5128=CARTESIAN_POINT('',(-0.750555349946514,0.,-9.19165206894919E-17));
#5129=CARTESIAN_POINT('',(-0.750555349946514,0.,-9.19165206894919E-17));
#5130=CARTESIAN_POINT('Origin',(-0.375277674973257,0.,-0.65));
#5131=CARTESIAN_POINT('',(-0.375277674973257,0.,-0.65));
#5132=CARTESIAN_POINT('Origin',(0.,0.53,-1.11022302462516E-16));
#5133=CARTESIAN_POINT('Origin',(0.,0.,-1.11022302462516E-16));
#5134=CARTESIAN_POINT('',(0.,0.,0.));
#5135=CARTESIAN_POINT('',(0.,-2.,1.));
#5136=CARTESIAN_POINT('',(2.5,-2.,1.42));
#5137=CARTESIAN_POINT('',(2.5,-2.,2.8));
#5138=CARTESIAN_POINT('',(2.5,-2.,2.9));
#5139=CARTESIAN_POINT('',(7.5,-2.,1.42));
#5140=CARTESIAN_POINT('',(7.5,-2.,2.8));
#5141=CARTESIAN_POINT('',(7.5,-2.,2.9));
#5142=CARTESIAN_POINT('',(5.,-0.96,8.));
#5143=CARTESIAN_POINT('',(0.,0.,0.));
#5144=CARTESIAN_POINT('',(0.,0.,0.));
#5145=CARTESIAN_POINT('Origin',(28.75,1.98,12.25));
#5146=CARTESIAN_POINT('',(28.42,2.08,12.25));
#5147=CARTESIAN_POINT('Origin',(28.75,2.08,12.25));
#5148=CARTESIAN_POINT('',(28.42,2.88,12.25));
#5149=CARTESIAN_POINT('',(28.42,1.98,12.25));
#5150=CARTESIAN_POINT('Origin',(28.75,2.88,12.25));
#5151=CARTESIAN_POINT('Origin',(21.25,1.98,19.75));
#5152=CARTESIAN_POINT('',(20.92,2.08,19.75));
#5153=CARTESIAN_POINT('Origin',(21.25,2.08,19.75));
#5154=CARTESIAN_POINT('',(20.92,2.88,19.75));
#5155=CARTESIAN_POINT('',(20.92,1.98,19.75));
#5156=CARTESIAN_POINT('Origin',(21.25,2.88,19.75));
#5157=CARTESIAN_POINT('Origin',(21.25,1.98,12.25));
#5158=CARTESIAN_POINT('',(20.92,2.08,12.25));
#5159=CARTESIAN_POINT('Origin',(21.25,2.08,12.25));
#5160=CARTESIAN_POINT('',(20.92,2.88,12.25));
#5161=CARTESIAN_POINT('',(20.92,1.98,12.25));
#5162=CARTESIAN_POINT('Origin',(21.25,2.88,12.25));
#5163=CARTESIAN_POINT('Origin',(28.75,1.98,19.75));
#5164=CARTESIAN_POINT('',(28.42,2.08,19.75));
#5165=CARTESIAN_POINT('Origin',(28.75,2.08,19.75));
#5166=CARTESIAN_POINT('',(28.42,2.88,19.75));
#5167=CARTESIAN_POINT('',(28.42,1.98,19.75));
#5168=CARTESIAN_POINT('Origin',(28.75,2.88,19.75));
#5169=CARTESIAN_POINT('Origin',(25.,1.98,8.));
#5170=CARTESIAN_POINT('',(24.575,2.08,8.));
#5171=CARTESIAN_POINT('Origin',(25.,2.08,8.));
#5172=CARTESIAN_POINT('',(24.575,2.88,8.));
#5173=CARTESIAN_POINT('',(24.575,1.98,8.));
#5174=CARTESIAN_POINT('Origin',(25.,2.88,8.));
#5175=CARTESIAN_POINT('Origin',(30.,2.08,11.));
#5176=CARTESIAN_POINT('',(26.,2.88,11.));
#5177=CARTESIAN_POINT('',(26.,2.08,11.));
#5178=CARTESIAN_POINT('',(26.,2.08,11.));
#5179=CARTESIAN_POINT('',(30.,2.88,11.));
#5180=CARTESIAN_POINT('',(20.,2.88,11.));
#5181=CARTESIAN_POINT('',(30.,2.08,11.));
#5182=CARTESIAN_POINT('',(30.,2.08,11.));
#5183=CARTESIAN_POINT('',(20.,2.08,11.));
#5184=CARTESIAN_POINT('Origin',(20.,2.08,11.));
#5185=CARTESIAN_POINT('',(20.,2.08,21.));
#5186=CARTESIAN_POINT('',(20.,2.08,11.));
#5187=CARTESIAN_POINT('',(20.,2.08,21.));
#5188=CARTESIAN_POINT('',(20.,2.88,21.));
#5189=CARTESIAN_POINT('',(20.,2.08,21.));
#5190=CARTESIAN_POINT('',(20.,2.88,11.));
#5191=CARTESIAN_POINT('',(20.,2.88,21.));
#5192=CARTESIAN_POINT('',(20.,2.08,11.));
#5193=CARTESIAN_POINT('Origin',(30.,2.08,11.));
#5194=CARTESIAN_POINT('',(24.,2.08,11.));
#5195=CARTESIAN_POINT('',(24.,2.88,11.));
#5196=CARTESIAN_POINT('',(24.,2.08,11.));
#5197=CARTESIAN_POINT('',(20.,2.08,11.));
#5198=CARTESIAN_POINT('',(20.,2.88,11.));
#5199=CARTESIAN_POINT('Origin',(30.,2.08,21.));
#5200=CARTESIAN_POINT('',(30.,2.08,21.));
#5201=CARTESIAN_POINT('',(30.,2.08,11.));
#5202=CARTESIAN_POINT('',(30.,2.88,21.));
#5203=CARTESIAN_POINT('',(30.,2.88,11.));
#5204=CARTESIAN_POINT('',(30.,2.08,21.));
#5205=CARTESIAN_POINT('Origin',(20.,2.08,21.));
#5206=CARTESIAN_POINT('',(30.,2.08,21.));
#5207=CARTESIAN_POINT('',(30.,2.88,21.));
#5208=CARTESIAN_POINT('Origin',(24.,2.08,8.));
#5209=CARTESIAN_POINT('',(24.,2.88,9.11803398874989));
#5210=CARTESIAN_POINT('',(24.,2.88,12.));
#5211=CARTESIAN_POINT('',(24.,2.08,9.11803398874989));
#5212=CARTESIAN_POINT('',(24.,2.08,9.11803398874989));
#5213=CARTESIAN_POINT('',(24.,2.08,12.));
#5214=CARTESIAN_POINT('Origin',(25.,2.88,8.));
#5215=CARTESIAN_POINT('',(26.,2.88,9.11803398874989));
#5216=CARTESIAN_POINT('',(26.,2.88,8.));
#5217=CARTESIAN_POINT('Origin',(25.,2.88,8.));
#5218=CARTESIAN_POINT('Origin',(26.,2.08,12.));
#5219=CARTESIAN_POINT('',(26.,2.08,9.11803398874989));
#5220=CARTESIAN_POINT('',(26.,2.08,8.));
#5221=CARTESIAN_POINT('',(26.,2.08,9.11803398874989));
#5222=CARTESIAN_POINT('Origin',(25.,2.08,8.));
#5223=CARTESIAN_POINT('Origin',(25.,2.08,8.));
#5224=CARTESIAN_POINT('Origin',(25.,2.08,8.));
#5225=CARTESIAN_POINT('',(0.,0.,0.));
#5226=CARTESIAN_POINT('Origin',(0.,0.,0.));
#5227=CARTESIAN_POINT('',(-0.42,0.16,5.14351655641888E-17));
#5228=CARTESIAN_POINT('Origin',(0.,0.16,0.));
#5229=CARTESIAN_POINT('',(-0.42,0.,5.14351655641888E-17));
#5230=CARTESIAN_POINT('',(-0.42,0.,5.14351655641888E-17));
#5231=CARTESIAN_POINT('Origin',(0.,0.,0.));
#5232=CARTESIAN_POINT('Origin',(0.,0.,0.));
#5233=CARTESIAN_POINT('',(-0.8,0.16,9.79717439317883E-17));
#5234=CARTESIAN_POINT('Origin',(0.,0.16,0.));
#5235=CARTESIAN_POINT('',(-0.8,0.,9.79717439317883E-17));
#5236=CARTESIAN_POINT('',(-0.8,0.,9.79717439317883E-17));
#5237=CARTESIAN_POINT('Origin',(0.,0.,0.));
#5238=CARTESIAN_POINT('Origin',(0.,0.16,0.));
#5239=CARTESIAN_POINT('Origin',(0.,0.,0.));
#5240=CARTESIAN_POINT('',(0.,0.,0.));
#5241=CARTESIAN_POINT('Origin',(0.,0.067277284513851,0.));
#5242=CARTESIAN_POINT('',(-0.375277674973257,0.0768195421087395,0.65));
#5243=CARTESIAN_POINT('',(0.375277674973257,0.0768195421087395,0.65));
#5244=CARTESIAN_POINT('Ctrl Pts',(-0.375277674973257,0.0768195421087395,
0.65));
#5245=CARTESIAN_POINT('Ctrl Pts',(1.66533453693773E-13,-0.0315137912242439,
0.65));
#5246=CARTESIAN_POINT('Ctrl Pts',(0.375277674973257,0.0768195421087394,
0.65));
#5247=CARTESIAN_POINT('',(-0.750555349946514,0.0768195421087394,-9.19165206894919E-17));
#5248=CARTESIAN_POINT('Ctrl Pts',(-0.750555349946514,0.0768195421087394,
-9.19165206894919E-17));
#5249=CARTESIAN_POINT('Ctrl Pts',(-0.562916512459802,-0.0315137912242434,
0.325000000000144));
#5250=CARTESIAN_POINT('Ctrl Pts',(-0.375277674973257,0.0768195421087395,
0.65));
#5251=CARTESIAN_POINT('',(-0.6175,-2.77555756156289E-17,-7.5621939847349E-17));
#5252=CARTESIAN_POINT('',(-0.734027674973257,0.067277284513851,-8.98924642641573E-17));
#5253=CARTESIAN_POINT('Origin',(0.,0.,0.));
#5254=CARTESIAN_POINT('',(-0.375277674973257,0.0768195421087395,-0.65));
#5255=CARTESIAN_POINT('Ctrl Pts',(-0.375277674973257,0.0768195421087395,
-0.65));
#5256=CARTESIAN_POINT('Ctrl Pts',(-0.562916512459968,-0.0315137912242437,
-0.324999999999856));
#5257=CARTESIAN_POINT('Ctrl Pts',(-0.750555349946514,0.0768195421087395,
-9.19165206894919E-17));
#5258=CARTESIAN_POINT('',(0.375277674973257,0.0768195421087395,-0.65));
#5259=CARTESIAN_POINT('Ctrl Pts',(0.375277674973257,0.0768195421087395,
-0.65));
#5260=CARTESIAN_POINT('Ctrl Pts',(-1.66144875635155E-13,-0.0315137912242437,
-0.65));
#5261=CARTESIAN_POINT('Ctrl Pts',(-0.375277674973257,0.0768195421087395,
-0.65));
#5262=CARTESIAN_POINT('',(0.750555349946514,0.0768195421087394,0.));
#5263=CARTESIAN_POINT('Ctrl Pts',(0.750555349946514,0.0768195421087394,
0.));
#5264=CARTESIAN_POINT('Ctrl Pts',(0.562916512459802,-0.0315137912242436,
-0.325000000000144));
#5265=CARTESIAN_POINT('Ctrl Pts',(0.375277674973257,0.0768195421087395,
-0.65));
#5266=CARTESIAN_POINT('Ctrl Pts',(0.375277674973257,0.0768195421087394,
0.65));
#5267=CARTESIAN_POINT('Ctrl Pts',(0.562916512459968,-0.0315137912242439,
0.324999999999856));
#5268=CARTESIAN_POINT('Ctrl Pts',(0.750555349946514,0.0768195421087394,
0.));
#5269=CARTESIAN_POINT('Origin',(0.,0.612722715486149,0.));
#5270=CARTESIAN_POINT('',(-0.6175,0.68,-7.5621939847349E-17));
#5271=CARTESIAN_POINT('Origin',(0.,0.68,0.));
#5272=CARTESIAN_POINT('',(-0.750555349946514,0.603180457891261,-9.19165206894919E-17));
#5273=CARTESIAN_POINT('',(-0.734027674973257,0.612722715486149,-8.98924642641573E-17));
#5274=CARTESIAN_POINT('',(-0.375277674973257,0.603180457891261,0.65));
#5275=CARTESIAN_POINT('Ctrl Pts',(-0.375277674973257,0.603180457891261,
0.65));
#5276=CARTESIAN_POINT('Ctrl Pts',(-0.562916512459968,0.711513791224243,
0.324999999999856));
#5277=CARTESIAN_POINT('Ctrl Pts',(-0.750555349946514,0.603180457891261,
-9.19165206894919E-17));
#5278=CARTESIAN_POINT('',(0.375277674973257,0.603180457891261,0.65));
#5279=CARTESIAN_POINT('Ctrl Pts',(0.375277674973257,0.603180457891261,0.65));
#5280=CARTESIAN_POINT('Ctrl Pts',(-1.66755498298699E-13,0.711513791224244,
0.65));
#5281=CARTESIAN_POINT('Ctrl Pts',(-0.375277674973257,0.603180457891261,
0.65));
#5282=CARTESIAN_POINT('',(0.750555349946514,0.603180457891261,0.));
#5283=CARTESIAN_POINT('Ctrl Pts',(0.750555349946514,0.603180457891261,0.));
#5284=CARTESIAN_POINT('Ctrl Pts',(0.562916512459802,0.711513791224244,0.325000000000144));
#5285=CARTESIAN_POINT('Ctrl Pts',(0.375277674973257,0.603180457891261,0.65));
#5286=CARTESIAN_POINT('',(0.375277674973257,0.603180457891261,-0.65));
#5287=CARTESIAN_POINT('Ctrl Pts',(0.375277674973257,0.603180457891261,-0.65));
#5288=CARTESIAN_POINT('Ctrl Pts',(0.562916512459969,0.711513791224244,-0.324999999999856));
#5289=CARTESIAN_POINT('Ctrl Pts',(0.750555349946514,0.603180457891261,0.));
#5290=CARTESIAN_POINT('',(-0.375277674973257,0.603180457891261,-0.65));
#5291=CARTESIAN_POINT('Ctrl Pts',(-0.375277674973257,0.603180457891261,
-0.65));
#5292=CARTESIAN_POINT('Ctrl Pts',(1.66422431391311E-13,0.711513791224244,
-0.65));
#5293=CARTESIAN_POINT('Ctrl Pts',(0.375277674973257,0.603180457891261,-0.65));
#5294=CARTESIAN_POINT('Ctrl Pts',(-0.750555349946514,0.603180457891261,
-9.19165206894919E-17));
#5295=CARTESIAN_POINT('Ctrl Pts',(-0.562916512459802,0.711513791224244,
-0.325000000000144));
#5296=CARTESIAN_POINT('Ctrl Pts',(-0.375277674973257,0.603180457891261,
-0.65));
#5297=CARTESIAN_POINT('Origin',(0.375277674973257,0.,-0.65));
#5298=CARTESIAN_POINT('',(-0.375277674973257,0.,-0.65));
#5299=CARTESIAN_POINT('',(0.375277674973257,0.,-0.65));
#5300=CARTESIAN_POINT('Origin',(-0.375277674973257,0.,-0.65));
#5301=CARTESIAN_POINT('',(-0.750555349946514,0.,-9.19165206894919E-17));
#5302=CARTESIAN_POINT('Origin',(-0.750555349946514,0.,-9.19165206894919E-17));
#5303=CARTESIAN_POINT('',(-0.375277674973257,0.,0.65));
#5304=CARTESIAN_POINT('Origin',(0.,0.,0.));
#5305=CARTESIAN_POINT('',(-0.338975,0.68,4.15124648740974E-17));
#5306=CARTESIAN_POINT('Origin',(0.,0.68,0.));
#5307=CARTESIAN_POINT('',(-0.338975,0.,4.15124648740974E-17));
#5308=CARTESIAN_POINT('',(-0.338975,0.,4.15124648740974E-17));
#5309=CARTESIAN_POINT('Origin',(0.,0.,0.));
#5310=CARTESIAN_POINT('Origin',(-0.375277674973257,0.,0.65));
#5311=CARTESIAN_POINT('',(0.375277674973257,0.,0.65));
#5312=CARTESIAN_POINT('Origin',(0.750555349946514,0.,0.));
#5313=CARTESIAN_POINT('',(0.750555349946514,0.,0.));
#5314=CARTESIAN_POINT('Origin',(0.375277674973257,0.,0.65));
#5315=CARTESIAN_POINT('Origin',(0.,0.68,-1.11022302462516E-16));
#5316=CARTESIAN_POINT('Origin',(0.,0.,-1.11022302462516E-16));
#5317=CARTESIAN_POINT('',(0.,0.,0.));
#5318=CARTESIAN_POINT('Origin',(6.5,-5.73205080756888,7.22132034));
#5319=CARTESIAN_POINT('',(6.89841665441537,-5.69649564641799,8.48132034));
#5320=CARTESIAN_POINT('',(6.89841665441537,-5.69649564641799,7.28132034));
#5321=CARTESIAN_POINT('',(6.89841665441537,-5.69649564641799,7.22132034));
#5322=CARTESIAN_POINT('',(6.33158334558463,-5.36923428297892,8.48132034));
#5323=CARTESIAN_POINT('Origin',(6.5,-5.73205080756888,8.48132034));
#5324=CARTESIAN_POINT('',(6.33158334558463,-5.36923428297892,7.28132034));
#5325=CARTESIAN_POINT('',(6.33158334558463,-5.36923428297892,7.22132034));
#5326=CARTESIAN_POINT('Origin',(6.5,-5.73205080756888,7.28132034));
#5327=CARTESIAN_POINT('Origin',(9.5,-4.,7.22132034));
#5328=CARTESIAN_POINT('',(9.27,-4.32726136343907,7.28132034));
#5329=CARTESIAN_POINT('',(9.27,-4.32726136343907,8.48132034));
#5330=CARTESIAN_POINT('',(9.27,-4.32726136343907,7.22132034));
#5331=CARTESIAN_POINT('',(9.27,-3.67273863656093,7.28132034));
#5332=CARTESIAN_POINT('Origin',(9.5,-4.,7.28132034));
#5333=CARTESIAN_POINT('',(9.27,-3.67273863656093,8.48132034));
#5334=CARTESIAN_POINT('',(9.27,-3.67273863656093,7.22132034));
#5335=CARTESIAN_POINT('Origin',(9.5,-4.,8.48132034));
#5336=CARTESIAN_POINT('Origin',(8.5,-2.26794919243112,7.22132034));
#5337=CARTESIAN_POINT('',(8.10158334558463,-2.30350435358201,8.48132034));
#5338=CARTESIAN_POINT('',(8.10158334558463,-2.30350435358201,7.28132034));
#5339=CARTESIAN_POINT('',(8.10158334558463,-2.30350435358201,7.22132034));
#5340=CARTESIAN_POINT('',(8.66841665441537,-2.63076571702108,8.48132034));
#5341=CARTESIAN_POINT('Origin',(8.5,-2.26794919243112,8.48132034));
#5342=CARTESIAN_POINT('',(8.66841665441537,-2.63076571702108,7.28132034));
#5343=CARTESIAN_POINT('',(8.66841665441537,-2.63076571702108,7.22132034));
#5344=CARTESIAN_POINT('Origin',(8.5,-2.26794919243112,7.28132034));
#5345=CARTESIAN_POINT('Origin',(6.5,-2.26794919243112,7.22132034));
#5346=CARTESIAN_POINT('',(6.33158334558463,-2.63076571702108,8.48132034));
#5347=CARTESIAN_POINT('',(6.33158334558463,-2.63076571702108,7.28132034));
#5348=CARTESIAN_POINT('',(6.33158334558463,-2.63076571702108,7.22132034));
#5349=CARTESIAN_POINT('',(6.89841665441537,-2.30350435358201,8.48132034));
#5350=CARTESIAN_POINT('Origin',(6.5,-2.26794919243112,8.48132034));
#5351=CARTESIAN_POINT('',(6.89841665441537,-2.30350435358201,7.28132034));
#5352=CARTESIAN_POINT('',(6.89841665441537,-2.30350435358201,7.22132034));
#5353=CARTESIAN_POINT('Origin',(6.5,-2.26794919243112,7.28132034));
#5354=CARTESIAN_POINT('Origin',(5.5,-4.,7.22132034));
#5355=CARTESIAN_POINT('',(5.73,-4.32726136343907,8.48132034));
#5356=CARTESIAN_POINT('',(5.73,-4.32726136343907,7.28132034));
#5357=CARTESIAN_POINT('',(5.73,-4.32726136343907,7.22132034));
#5358=CARTESIAN_POINT('',(5.73,-3.67273863656093,8.48132034));
#5359=CARTESIAN_POINT('Origin',(5.5,-4.,8.48132034));
#5360=CARTESIAN_POINT('',(5.73,-3.67273863656093,7.28132034));
#5361=CARTESIAN_POINT('',(5.73,-3.67273863656093,7.22132034));
#5362=CARTESIAN_POINT('Origin',(5.5,-4.,7.28132034));
#5363=CARTESIAN_POINT('Origin',(8.5,-5.73205080756888,7.22132034));
#5364=CARTESIAN_POINT('',(8.66841665441537,-5.36923428297892,8.48132034));
#5365=CARTESIAN_POINT('',(8.66841665441537,-5.36923428297892,7.28132034));
#5366=CARTESIAN_POINT('',(8.66841665441537,-5.36923428297892,7.22132034));
#5367=CARTESIAN_POINT('',(8.10158334558463,-5.69649564641799,8.48132034));
#5368=CARTESIAN_POINT('Origin',(8.5,-5.73205080756888,8.48132034));
#5369=CARTESIAN_POINT('',(8.10158334558463,-5.69649564641799,7.28132034));
#5370=CARTESIAN_POINT('',(8.10158334558463,-5.69649564641799,7.22132034));
#5371=CARTESIAN_POINT('Origin',(8.5,-5.73205080756888,7.28132034));
#5372=CARTESIAN_POINT('Origin',(7.5,-4.,8.48132034));
#5373=CARTESIAN_POINT('Origin',(7.5,-4.,8.48132034));
#5374=CARTESIAN_POINT('Origin',(7.5,-4.,8.48132034));
#5375=CARTESIAN_POINT('Origin',(7.5,-4.,8.48132034));
#5376=CARTESIAN_POINT('Origin',(7.5,-4.,8.48132034));
#5377=CARTESIAN_POINT('Origin',(7.5,-4.,8.48132034));
#5378=CARTESIAN_POINT('Origin',(7.5,-4.,8.48132034));
#5379=CARTESIAN_POINT('',(7.075,-4.,8.48132034));
#5380=CARTESIAN_POINT('Origin',(7.5,-4.,8.48132034));
#5381=CARTESIAN_POINT('Origin',(7.5,-4.,7.28132034));
#5382=CARTESIAN_POINT('Origin',(7.5,-4.,7.28132034));
#5383=CARTESIAN_POINT('Origin',(7.5,-4.,7.28132034));
#5384=CARTESIAN_POINT('Origin',(7.5,-4.,7.28132034));
#5385=CARTESIAN_POINT('Origin',(7.5,-4.,7.28132034));
#5386=CARTESIAN_POINT('Origin',(7.5,-4.,7.28132034));
#5387=CARTESIAN_POINT('Origin',(7.5,-4.,7.28132034));
#5388=CARTESIAN_POINT('Origin',(7.5,-4.,7.28132034));
#5389=CARTESIAN_POINT('Origin',(7.5,-4.,7.28132034));
#5390=CARTESIAN_POINT('Origin',(7.5,-4.,7.28132034));
#5391=CARTESIAN_POINT('Origin',(7.5,-4.,7.28132034));
#5392=CARTESIAN_POINT('Origin',(7.5,-4.,7.28132034));
#5393=CARTESIAN_POINT('Origin',(7.87527767497326,-3.35,7.27132034));
#5394=CARTESIAN_POINT('',(7.87527767497326,-3.35,7.28132034));
#5395=CARTESIAN_POINT('',(7.12472232502674,-3.35,7.28132034));
#5396=CARTESIAN_POINT('',(7.68763883748663,-3.35,7.28132034));
#5397=CARTESIAN_POINT('',(7.87527767497326,-3.35,7.97132034));
#5398=CARTESIAN_POINT('',(7.87527767497326,-3.35,7.27132034));
#5399=CARTESIAN_POINT('',(7.12472232502674,-3.35,7.97132034));
#5400=CARTESIAN_POINT('',(7.87527767497326,-3.35,7.97132034));
#5401=CARTESIAN_POINT('',(7.12472232502674,-3.35,7.27132034));
#5402=CARTESIAN_POINT('Origin',(7.12472232502674,-3.35,7.27132034));
#5403=CARTESIAN_POINT('',(6.74944465005349,-4.,7.28132034));
#5404=CARTESIAN_POINT('',(7.03090290628343,-3.5125,7.28132034));
#5405=CARTESIAN_POINT('',(6.74944465005349,-4.,7.97132034));
#5406=CARTESIAN_POINT('',(7.12472232502674,-3.35,7.97132034));
#5407=CARTESIAN_POINT('',(6.74944465005349,-4.,7.27132034));
#5408=CARTESIAN_POINT('Origin',(6.74944465005349,-4.,7.27132034));
#5409=CARTESIAN_POINT('',(7.12472232502674,-4.65,7.28132034));
#5410=CARTESIAN_POINT('',(6.8432640687968,-4.1625,7.28132034));
#5411=CARTESIAN_POINT('',(7.12472232502674,-4.65,7.97132034));
#5412=CARTESIAN_POINT('',(6.74944465005349,-4.,7.97132034));
#5413=CARTESIAN_POINT('',(7.12472232502674,-4.65,7.27132034));
#5414=CARTESIAN_POINT('Origin',(7.12472232502674,-4.65,7.27132034));
#5415=CARTESIAN_POINT('',(7.87527767497326,-4.65,7.28132034));
#5416=CARTESIAN_POINT('',(7.31236116251337,-4.65,7.28132034));
#5417=CARTESIAN_POINT('',(7.87527767497326,-4.65,7.97132034));
#5418=CARTESIAN_POINT('',(7.12472232502674,-4.65,7.97132034));
#5419=CARTESIAN_POINT('',(7.87527767497326,-4.65,7.27132034));
#5420=CARTESIAN_POINT('Origin',(8.25055534994651,-4.,7.27132034));
#5421=CARTESIAN_POINT('',(8.25055534994651,-4.,7.28132034));
#5422=CARTESIAN_POINT('',(8.1567359312032,-3.8375,7.28132034));
#5423=CARTESIAN_POINT('',(8.25055534994651,-4.,7.97132034));
#5424=CARTESIAN_POINT('',(8.25055534994651,-4.,7.27132034));
#5425=CARTESIAN_POINT('',(8.25055534994651,-4.,7.97132034));
#5426=CARTESIAN_POINT('Origin',(7.87527767497326,-4.65,7.27132034));
#5427=CARTESIAN_POINT('',(7.96909709371657,-4.4875,7.28132034));
#5428=CARTESIAN_POINT('',(7.87527767497326,-4.65,7.97132034));
#5429=CARTESIAN_POINT('Origin',(7.5,-4.,7.97132034));
#5430=CARTESIAN_POINT('',(7.075,-4.,7.97132034));
#5431=CARTESIAN_POINT('Origin',(7.5,-4.,7.97132034));
#5432=CARTESIAN_POINT('Origin',(7.5,-4.,7.28132034));
#5433=CARTESIAN_POINT('',(7.075,-4.,7.28132034));
#5434=CARTESIAN_POINT('Origin',(7.5,-4.,7.28132034));
#5435=CARTESIAN_POINT('',(0.,0.,0.));
#5436=CARTESIAN_POINT('',(5.,-0.96,8.));
#5437=CARTESIAN_POINT('',(5.,0.,8.));
#5438=CARTESIAN_POINT('',(5.,0.96,8.));
#5439=CARTESIAN_POINT('',(5.,1.12,8.));
#5440=CARTESIAN_POINT('',(-2.5,-6.16132034355964,4.));
#5441=CARTESIAN_POINT('',(15.,0.,8.));
#5442=CARTESIAN_POINT('',(10.,0.96,0.));
#5443=CARTESIAN_POINT('',(15.,0.,8.));
#5444=CARTESIAN_POINT('',(15.,0.96,8.));
#5445=CARTESIAN_POINT('',(15.,1.92,8.));
#5446=CARTESIAN_POINT('',(15.,2.08,8.));
#5447=CARTESIAN_POINT('',(7.5,-5.20132034355964,4.));
#5448=CARTESIAN_POINT('',(25.,0.96,8.));
#5449=CARTESIAN_POINT('',(0.,0.,0.));
#5450=CARTESIAN_POINT('',(25.,0.96,8.));
#5451=CARTESIAN_POINT('',(25.,1.92,8.));
#5452=CARTESIAN_POINT('',(25.,2.88,8.));
#5453=CARTESIAN_POINT('',(25.,3.04,8.));
#5454=CARTESIAN_POINT('',(17.5,-4.24132034355964,4.));
#5455=CARTESIAN_POINT('',(0.,0.,0.));
#5456=CARTESIAN_POINT('',(0.,0.,0.));
#5457=CARTESIAN_POINT('',(0.,0.,0.));
#5458=CARTESIAN_POINT('',(0.,0.,0.));
#5459=UNCERTAINTY_MEASURE_WITH_UNIT(LENGTH_MEASURE(0.001),#5493,
'DISTANCE_ACCURACY_VALUE',
'Maximum model space distance between geometric entities at asserted c
onnectivities');
#5460=UNCERTAINTY_MEASURE_WITH_UNIT(LENGTH_MEASURE(0.001),#5493,
'DISTANCE_ACCURACY_VALUE',
'Maximum model space distance between geometric entities at asserted c
onnectivities');
#5461=UNCERTAINTY_MEASURE_WITH_UNIT(LENGTH_MEASURE(0.001),#5493,
'DISTANCE_ACCURACY_VALUE',
'Maximum model space distance between geometric entities at asserted c
onnectivities');
#5462=UNCERTAINTY_MEASURE_WITH_UNIT(LENGTH_MEASURE(0.001),#5493,
'DISTANCE_ACCURACY_VALUE',
'Maximum model space distance between geometric entities at asserted c
onnectivities');
#5463=UNCERTAINTY_MEASURE_WITH_UNIT(LENGTH_MEASURE(0.001),#5493,
'DISTANCE_ACCURACY_VALUE',
'Maximum model space distance between geometric entities at asserted c
onnectivities');
#5464=UNCERTAINTY_MEASURE_WITH_UNIT(LENGTH_MEASURE(0.001),#5493,
'DISTANCE_ACCURACY_VALUE',
'Maximum model space distance between geometric entities at asserted c
onnectivities');
#5465=UNCERTAINTY_MEASURE_WITH_UNIT(LENGTH_MEASURE(0.001),#5493,
'DISTANCE_ACCURACY_VALUE',
'Maximum model space distance between geometric entities at asserted c
onnectivities');
#5466=UNCERTAINTY_MEASURE_WITH_UNIT(LENGTH_MEASURE(0.001),#5493,
'DISTANCE_ACCURACY_VALUE',
'Maximum model space distance between geometric entities at asserted c
onnectivities');
#5467=UNCERTAINTY_MEASURE_WITH_UNIT(LENGTH_MEASURE(0.001),#5493,
'DISTANCE_ACCURACY_VALUE',
'Maximum model space distance between geometric entities at asserted c
onnectivities');
#5468=UNCERTAINTY_MEASURE_WITH_UNIT(LENGTH_MEASURE(0.001),#5493,
'DISTANCE_ACCURACY_VALUE',
'Maximum model space distance between geometric entities at asserted c
onnectivities');
#5469=UNCERTAINTY_MEASURE_WITH_UNIT(LENGTH_MEASURE(0.001),#5493,
'DISTANCE_ACCURACY_VALUE',
'Maximum model space distance between geometric entities at asserted c
onnectivities');
#5470=UNCERTAINTY_MEASURE_WITH_UNIT(LENGTH_MEASURE(0.001),#5493,
'DISTANCE_ACCURACY_VALUE',
'Maximum model space distance between geometric entities at asserted c
onnectivities');
#5471=UNCERTAINTY_MEASURE_WITH_UNIT(LENGTH_MEASURE(0.001),#5493,
'DISTANCE_ACCURACY_VALUE',
'Maximum model space distance between geometric entities at asserted c
onnectivities');
#5472=UNCERTAINTY_MEASURE_WITH_UNIT(LENGTH_MEASURE(0.001),#5493,
'DISTANCE_ACCURACY_VALUE',
'Maximum model space distance between geometric entities at asserted c
onnectivities');
#5473=UNCERTAINTY_MEASURE_WITH_UNIT(LENGTH_MEASURE(0.001),#5493,
'DISTANCE_ACCURACY_VALUE',
'Maximum model space distance between geometric entities at asserted c
onnectivities');
#5474=UNCERTAINTY_MEASURE_WITH_UNIT(LENGTH_MEASURE(0.001),#5493,
'DISTANCE_ACCURACY_VALUE',
'Maximum model space distance between geometric entities at asserted c
onnectivities');
#5475=UNCERTAINTY_MEASURE_WITH_UNIT(LENGTH_MEASURE(0.001),#5493,
'DISTANCE_ACCURACY_VALUE',
'Maximum model space distance between geometric entities at asserted c
onnectivities');
#5476=(
GEOMETRIC_REPRESENTATION_CONTEXT(3)
GLOBAL_UNCERTAINTY_ASSIGNED_CONTEXT((#5459))
GLOBAL_UNIT_ASSIGNED_CONTEXT((#5493,#5495,#5496))
REPRESENTATION_CONTEXT('','3D')
);
#5477=(
GEOMETRIC_REPRESENTATION_CONTEXT(3)
GLOBAL_UNCERTAINTY_ASSIGNED_CONTEXT((#5460))
GLOBAL_UNIT_ASSIGNED_CONTEXT((#5493,#5495,#5496))
REPRESENTATION_CONTEXT('','3D')
);
#5478=(
GEOMETRIC_REPRESENTATION_CONTEXT(3)
GLOBAL_UNCERTAINTY_ASSIGNED_CONTEXT((#5461))
GLOBAL_UNIT_ASSIGNED_CONTEXT((#5493,#5495,#5496))
REPRESENTATION_CONTEXT('','3D')
);
#5479=(
GEOMETRIC_REPRESENTATION_CONTEXT(3)
GLOBAL_UNCERTAINTY_ASSIGNED_CONTEXT((#5462))
GLOBAL_UNIT_ASSIGNED_CONTEXT((#5493,#5495,#5496))
REPRESENTATION_CONTEXT('','3D')
);
#5480=(
GEOMETRIC_REPRESENTATION_CONTEXT(3)
GLOBAL_UNCERTAINTY_ASSIGNED_CONTEXT((#5463))
GLOBAL_UNIT_ASSIGNED_CONTEXT((#5493,#5495,#5496))
REPRESENTATION_CONTEXT('','3D')
);
#5481=(
GEOMETRIC_REPRESENTATION_CONTEXT(3)
GLOBAL_UNCERTAINTY_ASSIGNED_CONTEXT((#5464))
GLOBAL_UNIT_ASSIGNED_CONTEXT((#5493,#5495,#5496))
REPRESENTATION_CONTEXT('','3D')
);
#5482=(
GEOMETRIC_REPRESENTATION_CONTEXT(3)
GLOBAL_UNCERTAINTY_ASSIGNED_CONTEXT((#5465))
GLOBAL_UNIT_ASSIGNED_CONTEXT((#5493,#5495,#5496))
REPRESENTATION_CONTEXT('','3D')
);
#5483=(
GEOMETRIC_REPRESENTATION_CONTEXT(3)
GLOBAL_UNCERTAINTY_ASSIGNED_CONTEXT((#5466))
GLOBAL_UNIT_ASSIGNED_CONTEXT((#5493,#5495,#5496))
REPRESENTATION_CONTEXT('','3D')
);
#5484=(
GEOMETRIC_REPRESENTATION_CONTEXT(3)
GLOBAL_UNCERTAINTY_ASSIGNED_CONTEXT((#5467))
GLOBAL_UNIT_ASSIGNED_CONTEXT((#5493,#5495,#5496))
REPRESENTATION_CONTEXT('','3D')
);
#5485=(
GEOMETRIC_REPRESENTATION_CONTEXT(3)
GLOBAL_UNCERTAINTY_ASSIGNED_CONTEXT((#5468))
GLOBAL_UNIT_ASSIGNED_CONTEXT((#5493,#5495,#5496))
REPRESENTATION_CONTEXT('','3D')
);
#5486=(
GEOMETRIC_REPRESENTATION_CONTEXT(3)
GLOBAL_UNCERTAINTY_ASSIGNED_CONTEXT((#5469))
GLOBAL_UNIT_ASSIGNED_CONTEXT((#5493,#5495,#5496))
REPRESENTATION_CONTEXT('','3D')
);
#5487=(
GEOMETRIC_REPRESENTATION_CONTEXT(3)
GLOBAL_UNCERTAINTY_ASSIGNED_CONTEXT((#5470))
GLOBAL_UNIT_ASSIGNED_CONTEXT((#5493,#5495,#5496))
REPRESENTATION_CONTEXT('','3D')
);
#5488=(
GEOMETRIC_REPRESENTATION_CONTEXT(3)
GLOBAL_UNCERTAINTY_ASSIGNED_CONTEXT((#5471))
GLOBAL_UNIT_ASSIGNED_CONTEXT((#5493,#5495,#5496))
REPRESENTATION_CONTEXT('','3D')
);
#5489=(
GEOMETRIC_REPRESENTATION_CONTEXT(3)
GLOBAL_UNCERTAINTY_ASSIGNED_CONTEXT((#5472))
GLOBAL_UNIT_ASSIGNED_CONTEXT((#5493,#5495,#5496))
REPRESENTATION_CONTEXT('','3D')
);
#5490=(
GEOMETRIC_REPRESENTATION_CONTEXT(3)
GLOBAL_UNCERTAINTY_ASSIGNED_CONTEXT((#5473))
GLOBAL_UNIT_ASSIGNED_CONTEXT((#5493,#5495,#5496))
REPRESENTATION_CONTEXT('','3D')
);
#5491=(
GEOMETRIC_REPRESENTATION_CONTEXT(3)
GLOBAL_UNCERTAINTY_ASSIGNED_CONTEXT((#5474))
GLOBAL_UNIT_ASSIGNED_CONTEXT((#5493,#5495,#5496))
REPRESENTATION_CONTEXT('','3D')
);
#5492=(
GEOMETRIC_REPRESENTATION_CONTEXT(3)
GLOBAL_UNCERTAINTY_ASSIGNED_CONTEXT((#5475))
GLOBAL_UNIT_ASSIGNED_CONTEXT((#5493,#5495,#5496))
REPRESENTATION_CONTEXT('','3D')
);
#5493=(
LENGTH_UNIT()
NAMED_UNIT(*)
SI_UNIT(.CENTI.,.METRE.)
);
#5494=(
LENGTH_UNIT()
NAMED_UNIT(*)
SI_UNIT($,.METRE.)
);
#5495=(
NAMED_UNIT(*)
PLANE_ANGLE_UNIT()
SI_UNIT($,.RADIAN.)
);
#5496=(
NAMED_UNIT(*)
SI_UNIT($,.STERADIAN.)
SOLID_ANGLE_UNIT()
);
#5497=SHAPE_DEFINITION_REPRESENTATION(#5513,#5562);
#5498=SHAPE_DEFINITION_REPRESENTATION(#5514,#5563);
#5499=SHAPE_DEFINITION_REPRESENTATION(#5515,#5564);
#5500=SHAPE_DEFINITION_REPRESENTATION(#5516,#5565);
#5501=SHAPE_DEFINITION_REPRESENTATION(#5517,#5566);
#5502=SHAPE_DEFINITION_REPRESENTATION(#5518,#5567);
#5503=SHAPE_DEFINITION_REPRESENTATION(#5519,#5568);
#5504=SHAPE_DEFINITION_REPRESENTATION(#5520,#5569);
#5505=SHAPE_DEFINITION_REPRESENTATION(#5521,#5570);
#5506=SHAPE_DEFINITION_REPRESENTATION(#5522,#5571);
#5507=SHAPE_DEFINITION_REPRESENTATION(#5523,#5572);
#5508=SHAPE_DEFINITION_REPRESENTATION(#5533,#5573);
#5509=SHAPE_DEFINITION_REPRESENTATION(#5534,#5574);
#5510=SHAPE_DEFINITION_REPRESENTATION(#5535,#5575);
#5511=SHAPE_DEFINITION_REPRESENTATION(#5536,#5576);
#5512=SHAPE_DEFINITION_REPRESENTATION(#5537,#5577);
#5513=PRODUCT_DEFINITION_SHAPE('',$,#5579);
#5514=PRODUCT_DEFINITION_SHAPE('',$,#5580);
#5515=PRODUCT_DEFINITION_SHAPE('',$,#5581);
#5516=PRODUCT_DEFINITION_SHAPE('',$,#5582);
#5517=PRODUCT_DEFINITION_SHAPE('',$,#5583);
#5518=PRODUCT_DEFINITION_SHAPE('',$,#5584);
#5519=PRODUCT_DEFINITION_SHAPE('',$,#5585);
#5520=PRODUCT_DEFINITION_SHAPE('',$,#5586);
#5521=PRODUCT_DEFINITION_SHAPE('',$,#5587);
#5522=PRODUCT_DEFINITION_SHAPE('',$,#5588);
#5523=PRODUCT_DEFINITION_SHAPE('',$,#5589);
#5524=PRODUCT_DEFINITION_SHAPE($,$,#110);
#5525=PRODUCT_DEFINITION_SHAPE($,$,#111);
#5526=PRODUCT_DEFINITION_SHAPE($,$,#112);
#5527=PRODUCT_DEFINITION_SHAPE($,$,#113);
#5528=PRODUCT_DEFINITION_SHAPE($,$,#114);
#5529=PRODUCT_DEFINITION_SHAPE($,$,#115);
#5530=PRODUCT_DEFINITION_SHAPE($,$,#116);
#5531=PRODUCT_DEFINITION_SHAPE($,$,#117);
#5532=PRODUCT_DEFINITION_SHAPE($,$,#118);
#5533=PRODUCT_DEFINITION_SHAPE('',$,#5590);
#5534=PRODUCT_DEFINITION_SHAPE('',$,#5591);
#5535=PRODUCT_DEFINITION_SHAPE('',$,#5592);
#5536=PRODUCT_DEFINITION_SHAPE('',$,#5593);
#5537=PRODUCT_DEFINITION_SHAPE('',$,#5594);
#5538=PRODUCT_DEFINITION_SHAPE($,$,#119);
#5539=PRODUCT_DEFINITION_SHAPE($,$,#120);
#5540=PRODUCT_DEFINITION_SHAPE($,$,#121);
#5541=PRODUCT_DEFINITION_SHAPE($,$,#122);
#5542=PRODUCT_DEFINITION_SHAPE($,$,#123);
#5543=PRODUCT_DEFINITION_SHAPE($,$,#124);
#5544=PRODUCT_DEFINITION_SHAPE($,$,#125);
#5545=PRODUCT_DEFINITION_SHAPE($,$,#126);
#5546=PRODUCT_DEFINITION_SHAPE($,$,#127);
#5547=PRODUCT_DEFINITION_SHAPE($,$,#128);
#5548=PRODUCT_DEFINITION_SHAPE($,$,#129);
#5549=PRODUCT_DEFINITION_SHAPE($,$,#130);
#5550=PRODUCT_DEFINITION_SHAPE($,$,#131);
#5551=PRODUCT_DEFINITION_SHAPE($,$,#132);
#5552=PRODUCT_DEFINITION_SHAPE($,$,#133);
#5553=PRODUCT_DEFINITION_SHAPE($,$,#134);
#5554=PRODUCT_DEFINITION_SHAPE($,$,#135);
#5555=PRODUCT_DEFINITION_SHAPE($,$,#136);
#5556=PRODUCT_DEFINITION_SHAPE($,$,#137);
#5557=PRODUCT_DEFINITION_SHAPE($,$,#138);
#5558=PRODUCT_DEFINITION_SHAPE($,$,#139);
#5559=PRODUCT_DEFINITION_SHAPE($,$,#140);
#5560=PRODUCT_DEFINITION_SHAPE($,$,#141);
#5561=PRODUCT_DEFINITION_SHAPE($,$,#142);
#5562=SHAPE_REPRESENTATION('',(#3305,#3601,#3602,#3603,#3604),#5476);
#5563=SHAPE_REPRESENTATION('',(#3306,#3469,#3470,#3471,#3472,#3473,#3474,
#3475,#3476,#3477),#5477);
#5564=SHAPE_REPRESENTATION('',(#3307),#5478);
#5565=SHAPE_REPRESENTATION('',(#3327),#5479);
#5566=SHAPE_REPRESENTATION('',(#3377),#5480);
#5567=SHAPE_REPRESENTATION('',(#3398),#5481);
#5568=SHAPE_REPRESENTATION('',(#3409),#5482);
#5569=SHAPE_REPRESENTATION('',(#3433,#3581,#3582,#3583,#3584,#3585,#3586,
#3587),#5483);
#5570=SHAPE_REPRESENTATION('',(#3434,#3588,#3589,#3590,#3591,#3592,#3593,
#3594),#5484);
#5571=SHAPE_REPRESENTATION('',(#3435),#5485);
#5572=SHAPE_REPRESENTATION('',(#3452),#5486);
#5573=SHAPE_REPRESENTATION('',(#3478,#3595,#3596,#3597,#3598,#3599,#3600),
#5487);
#5574=SHAPE_REPRESENTATION('',(#3479),#5488);
#5575=SHAPE_REPRESENTATION('',(#3507),#5489);
#5576=SHAPE_REPRESENTATION('',(#3516),#5490);
#5577=SHAPE_REPRESENTATION('',(#3532),#5491);
#5578=PRODUCT_DEFINITION_CONTEXT('part definition',#5628,'design');
#5579=PRODUCT_DEFINITION('PAT-113','PAT-113',#5595,
#5578);
#5580=PRODUCT_DEFINITION('Rail and mounting bracket',
'Rail and mounting bracket',#5596,#5578);
#5581=PRODUCT_DEFINITION('Arm mounting bracket','Arm mounting bracket',
#5597,#5578);
#5582=PRODUCT_DEFINITION('Slotted Extrusion - 20 x 20 x 100 mm',
'Slotted Extrusion - 20 x 20 x 100 mm',#5598,#5578);
#5583=PRODUCT_DEFINITION('Captive slot nut','Captive slot nut',#5599,#5578);
#5584=PRODUCT_DEFINITION('Flat Washer - M5','Flat Washer - M5',#5600,#5578);
#5585=PRODUCT_DEFINITION('M5x14 Cap Screw','M5x14 Cap Screw',#5601,#5578);
#5586=PRODUCT_DEFINITION('Inner arm','Inner arm',#5602,#5578);
#5587=PRODUCT_DEFINITION('Outer arm','Outer arm',#5603,#5578);
#5588=PRODUCT_DEFINITION('Pivot link','Pivot link',#5604,#5578);
#5589=PRODUCT_DEFINITION('Hex Bolt - M8x40','Hex Bolt - M8x40',#5605,#5578);
#5590=PRODUCT_DEFINITION('Screen mounting plate',
'Screen mounting plate',#5606,#5578);
#5591=PRODUCT_DEFINITION('Screen mounting plate (1)',
'Screen mounting plate (1)',#5607,#5578);
#5592=PRODUCT_DEFINITION('Flat Washer - M8','Flat Washer - M8',#5608,#5578);
#5593=PRODUCT_DEFINITION('Hex Nut - M8','Hex Nut - M8',#5609,#5578);
#5594=PRODUCT_DEFINITION('Captive-nut hand knob',
'Captive-nut hand knob',#5610,#5578);
#5595=PRODUCT_DEFINITION_FORMATION('',$,#5630);
#5596=PRODUCT_DEFINITION_FORMATION('',$,#5631);
#5597=PRODUCT_DEFINITION_FORMATION('',$,#5632);
#5598=PRODUCT_DEFINITION_FORMATION('',$,#5633);
#5599=PRODUCT_DEFINITION_FORMATION('',$,#5634);
#5600=PRODUCT_DEFINITION_FORMATION('',$,#5635);
#5601=PRODUCT_DEFINITION_FORMATION('',$,#5636);
#5602=PRODUCT_DEFINITION_FORMATION('',$,#5637);
#5603=PRODUCT_DEFINITION_FORMATION('',$,#5638);
#5604=PRODUCT_DEFINITION_FORMATION('',$,#5639);
#5605=PRODUCT_DEFINITION_FORMATION('',$,#5640);
#5606=PRODUCT_DEFINITION_FORMATION('',$,#5641);
#5607=PRODUCT_DEFINITION_FORMATION('',$,#5642);
#5608=PRODUCT_DEFINITION_FORMATION('',$,#5643);
#5609=PRODUCT_DEFINITION_FORMATION('',$,#5644);
#5610=PRODUCT_DEFINITION_FORMATION('',$,#5645);
#5611=PRODUCT_RELATED_PRODUCT_CATEGORY('PAT-113','PAT-113',(#5630));
#5612=PRODUCT_RELATED_PRODUCT_CATEGORY('Rail and mounting bracket',
'Rail and mounting bracket',(#5631));
#5613=PRODUCT_RELATED_PRODUCT_CATEGORY('Arm mounting bracket',
'Arm mounting bracket',(#5632));
#5614=PRODUCT_RELATED_PRODUCT_CATEGORY(
'Slotted Extrusion - 20 x 20 x 100 mm',
'Slotted Extrusion - 20 x 20 x 100 mm',(#5633));
#5615=PRODUCT_RELATED_PRODUCT_CATEGORY('Captive slot nut',
'Captive slot nut',(#5634));
#5616=PRODUCT_RELATED_PRODUCT_CATEGORY('Flat Washer - M5',
'Flat Washer - M5',(#5635));
#5617=PRODUCT_RELATED_PRODUCT_CATEGORY('M5x14 Cap Screw',
'M5x14 Cap Screw',(#5636));
#5618=PRODUCT_RELATED_PRODUCT_CATEGORY('Inner arm','Inner arm',(#5637));
#5619=PRODUCT_RELATED_PRODUCT_CATEGORY('Outer arm','Outer arm',(#5638));
#5620=PRODUCT_RELATED_PRODUCT_CATEGORY('Pivot link','Pivot link',(#5639));
#5621=PRODUCT_RELATED_PRODUCT_CATEGORY('Hex Bolt - M8x40',
'Hex Bolt - M8x40',(#5640));
#5622=PRODUCT_RELATED_PRODUCT_CATEGORY('Screen mounting plate',
'Screen mounting plate',(#5641));
#5623=PRODUCT_RELATED_PRODUCT_CATEGORY('Screen mounting plate (1)',
'Screen mounting plate (1)',(#5642));
#5624=PRODUCT_RELATED_PRODUCT_CATEGORY('Flat Washer - M8',
'Flat Washer - M8',(#5643));
#5625=PRODUCT_RELATED_PRODUCT_CATEGORY('Hex Nut - M8','Hex Nut - M8',(#5644));
#5626=PRODUCT_RELATED_PRODUCT_CATEGORY('Captive-nut hand knob',
'Captive-nut hand knob',(#5645));
#5627=APPLICATION_PROTOCOL_DEFINITION('international standard',
'automotive_design',2009,#5628);
#5628=APPLICATION_CONTEXT(
'Core Data for Automotive Mechanical Design Process');
#5629=PRODUCT_CONTEXT('part definition',#5628,'mechanical');
#5630=PRODUCT('PAT-113','PAT-113',
'PAT-113',(#5629));
#5631=PRODUCT('Rail and mounting bracket','Rail and mounting bracket',
'Rail and mounting bracket',(#5629));
#5632=PRODUCT('Arm mounting bracket','Arm mounting bracket',
'Arm mounting bracket',(#5629));
#5633=PRODUCT('Slotted Extrusion - 20 x 20 x 100 mm',
'Slotted Extrusion - 20 x 20 x 100 mm',
'Slotted Extrusion - 20 x 20 x 100 mm',(#5629));
#5634=PRODUCT('Captive slot nut','Captive slot nut','Captive slot nut',
(#5629));
#5635=PRODUCT('Flat Washer - M5','Flat Washer - M5','Flat Washer - M5',
(#5629));
#5636=PRODUCT('M5x14 Cap Screw','M5x14 Cap Screw','M5x14 Cap Screw',(#5629));
#5637=PRODUCT('Inner arm','Inner arm','Inner arm',(#5629));
#5638=PRODUCT('Outer arm','Outer arm','Outer arm',(#5629));
#5639=PRODUCT('Pivot link','Pivot link','Pivot link',(#5629));
#5640=PRODUCT('Hex Bolt - M8x40','Hex Bolt - M8x40','Hex Bolt - M8x40',
(#5629));
#5641=PRODUCT('Screen mounting plate','Screen mounting plate',
'Screen mounting plate',(#5629));
#5642=PRODUCT('Screen mounting plate (1)','Screen mounting plate (1)',
'Screen mounting plate (1)',(#5629));
#5643=PRODUCT('Flat Washer - M8','Flat Washer - M8','Flat Washer - M8',
(#5629));
#5644=PRODUCT('Hex Nut - M8','Hex Nut - M8','Hex Nut - M8',(#5629));
#5645=PRODUCT('Captive-nut hand knob','Captive-nut hand knob',
'Captive-nut hand knob',(#5629));
#5646=PRESENTATION_STYLE_ASSIGNMENT((#5650));
#5647=PRESENTATION_STYLE_ASSIGNMENT((#5651));
#5648=PRESENTATION_STYLE_ASSIGNMENT((#5652));
#5649=PRESENTATION_STYLE_ASSIGNMENT((#5653));
#5650=SURFACE_STYLE_USAGE(.BOTH.,#5654);
#5651=SURFACE_STYLE_USAGE(.BOTH.,#5655);
#5652=SURFACE_STYLE_USAGE(.BOTH.,#5656);
#5653=SURFACE_STYLE_USAGE(.BOTH.,#5657);
#5654=SURFACE_SIDE_STYLE('',(#5658));
#5655=SURFACE_SIDE_STYLE('',(#5659));
#5656=SURFACE_SIDE_STYLE('',(#5660));
#5657=SURFACE_SIDE_STYLE('',(#5661));
#5658=SURFACE_STYLE_FILL_AREA(#5662);
#5659=SURFACE_STYLE_FILL_AREA(#5663);
#5660=SURFACE_STYLE_FILL_AREA(#5664);
#5661=SURFACE_STYLE_FILL_AREA(#5665);
#5662=FILL_AREA_STYLE('Steel - Satin',(#5666));
#5663=FILL_AREA_STYLE('CAD Library Painted - Engineering blue',(#5667));
#5664=FILL_AREA_STYLE('CAD Library Painted - Steel gray',(#5668));
#5665=FILL_AREA_STYLE('CAD Library Painted - Graphite',(#5669));
#5666=FILL_AREA_STYLE_COLOUR('Steel - Satin',#5670);
#5667=FILL_AREA_STYLE_COLOUR('CAD Library Painted - Engineering blue',#5671);
#5668=FILL_AREA_STYLE_COLOUR('CAD Library Painted - Steel gray',#5672);
#5669=FILL_AREA_STYLE_COLOUR('CAD Library Painted - Graphite',#5673);
#5670=COLOUR_RGB('Steel - Satin',0.627450980392157,0.627450980392157,0.627450980392157);
#5671=COLOUR_RGB('CAD Library Painted - Engineering blue',0.12156862745098,
0.356862745098039,0.6);
#5672=COLOUR_RGB('CAD Library Painted - Steel gray',0.592156862745098,0.631372549019608,
0.67843137254902);
#5673=COLOUR_RGB('CAD Library Painted - Graphite',0.0980392156862745,0.109803921568627,
0.125490196078431);
#5674=COLOUR_RGB('Dark Blue',0.08,0.2,0.34);
#5675=FILL_AREA_STYLE_COLOUR('',#5674);
#5676=FILL_AREA_STYLE('',(#5675));
#5677=SURFACE_STYLE_FILL_AREA(#5676);
#5678=SURFACE_SIDE_STYLE('',(#5677));
#5679=SURFACE_STYLE_USAGE(.BOTH.,#5678);
#5680=PRESENTATION_STYLE_ASSIGNMENT((#5679));
#5681=COLOUR_RGB('Light Blue',0.38,0.62,0.78);
#5682=FILL_AREA_STYLE_COLOUR('',#5681);
#5683=FILL_AREA_STYLE('',(#5682));
#5684=SURFACE_STYLE_FILL_AREA(#5683);
#5685=SURFACE_SIDE_STYLE('',(#5684));
#5686=SURFACE_STYLE_USAGE(.BOTH.,#5685);
#5687=PRESENTATION_STYLE_ASSIGNMENT((#5686));
#5688=COLOUR_RGB('Sky Blue',0.24,0.69,0.87);
#5689=FILL_AREA_STYLE_COLOUR('',#5688);
#5690=FILL_AREA_STYLE('',(#5689));
#5691=SURFACE_STYLE_FILL_AREA(#5690);
#5692=SURFACE_SIDE_STYLE('',(#5691));
#5693=SURFACE_STYLE_USAGE(.BOTH.,#5692);
#5694=PRESENTATION_STYLE_ASSIGNMENT((#5693));
#5695=COLOUR_RGB('Grey',0.48,0.52,0.57);
#5696=FILL_AREA_STYLE_COLOUR('',#5695);
#5697=FILL_AREA_STYLE('',(#5696));
#5698=SURFACE_STYLE_FILL_AREA(#5697);
#5699=SURFACE_SIDE_STYLE('',(#5698));
#5700=SURFACE_STYLE_USAGE(.BOTH.,#5699);
#5701=PRESENTATION_STYLE_ASSIGNMENT((#5700));
#5702=COLOUR_RGB('Black',0.12,0.14,0.17);
#5703=FILL_AREA_STYLE_COLOUR('',#5702);
#5704=FILL_AREA_STYLE('',(#5703));
#5705=SURFACE_STYLE_FILL_AREA(#5704);
#5706=SURFACE_SIDE_STYLE('',(#5705));
#5707=SURFACE_STYLE_USAGE(.BOTH.,#5706);
#5708=PRESENTATION_STYLE_ASSIGNMENT((#5707));
#5709=COLOUR_RGB('Off White',0.89,0.88,0.83);
#5710=FILL_AREA_STYLE_COLOUR('',#5709);
#5711=FILL_AREA_STYLE('',(#5710));
#5712=SURFACE_STYLE_FILL_AREA(#5711);
#5713=SURFACE_SIDE_STYLE('',(#5712));
#5714=SURFACE_STYLE_USAGE(.BOTH.,#5713);
#5715=PRESENTATION_STYLE_ASSIGNMENT((#5714));
ENDSEC;
END-ISO-10303-21;
